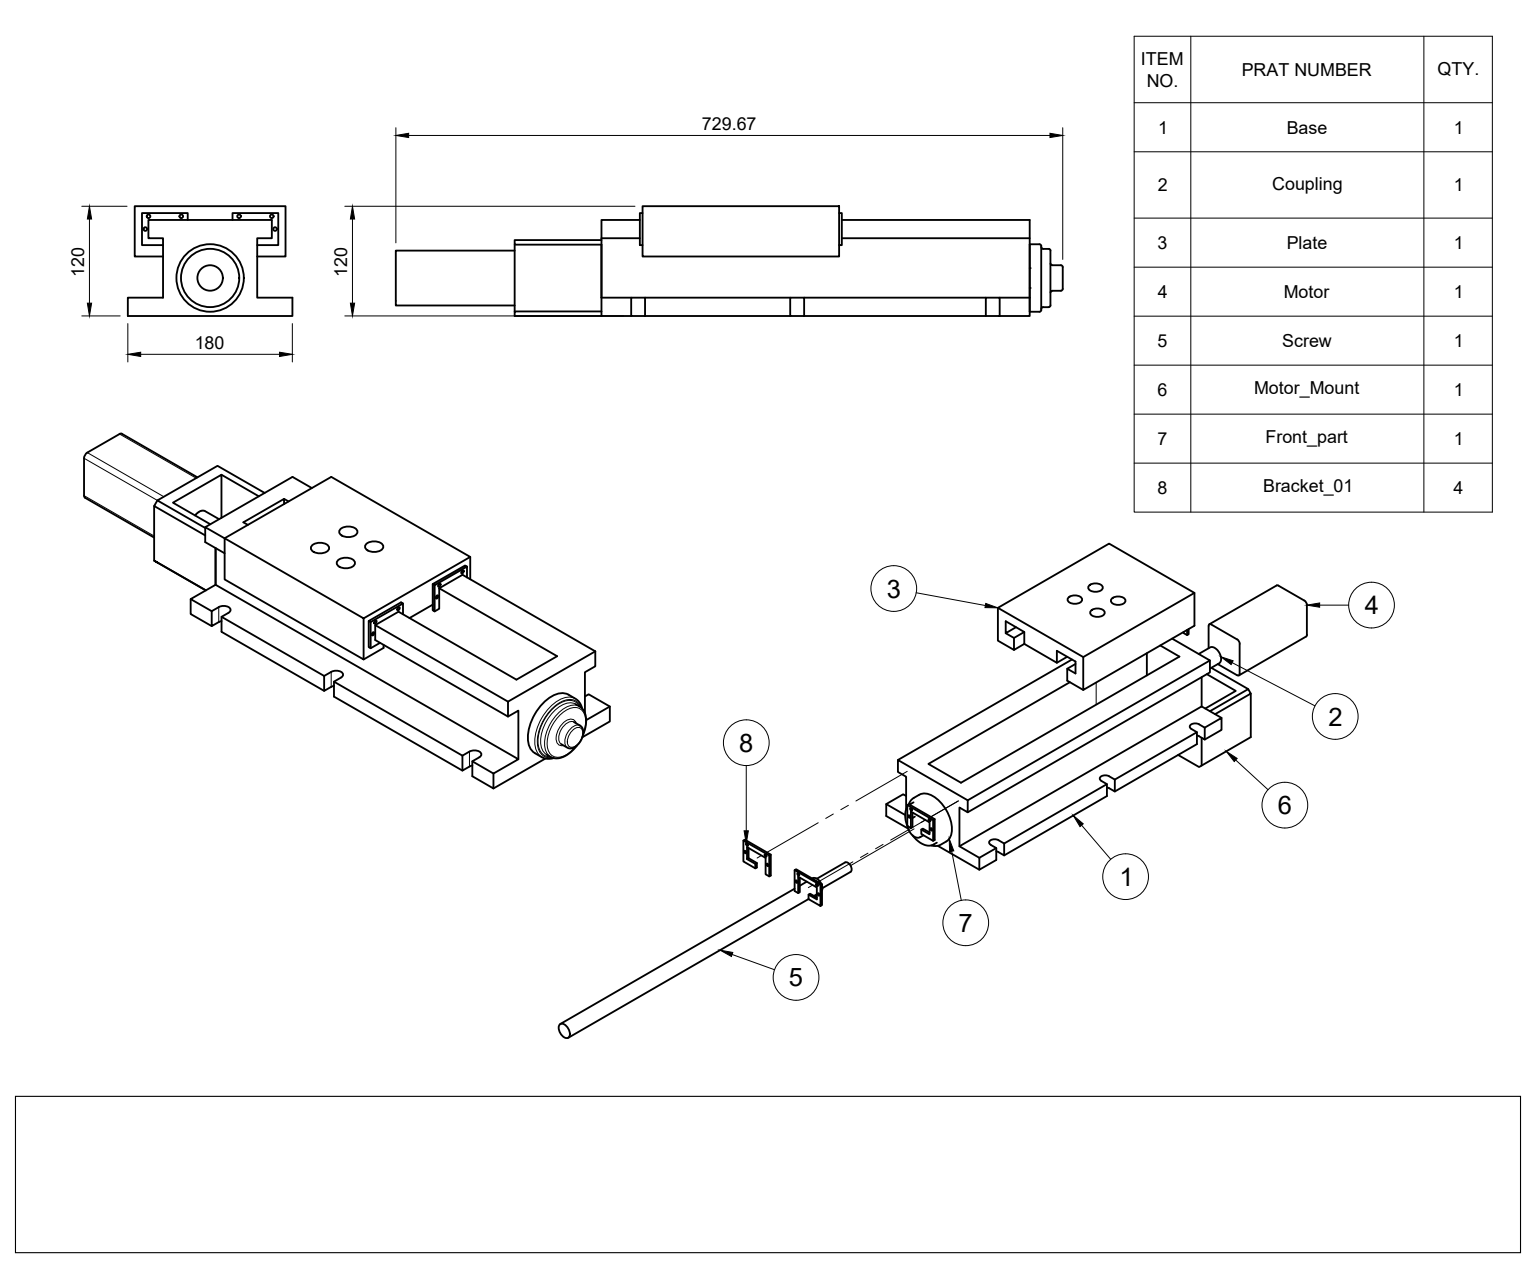
ISO-10303-21;
HEADER;
/* Generated by software containing ST-Developer
 * from STEP Tools, Inc. (www.steptools.com) 
 */

FILE_DESCRIPTION(
/* description */ (''),
/* implementation_level */ '2;1');

FILE_NAME(
/* name */ 'MAS-277',
/* time_stamp */ '2026-10-22T16:03:28+06:00',
/* author */ (''),
/* organization */ (''),
/* preprocessor_version */ 'ST-DEVELOPER v20.2',
/* originating_system */ 'Autodesk Translation Framework v15.15.0.0',
/* authorisation */ '');

FILE_SCHEMA (('AUTOMOTIVE_DESIGN { 1 0 10303 214 3 1 1 }'));
ENDSEC;

DATA;
#10=MECHANICAL_DESIGN_GEOMETRIC_PRESENTATION_REPRESENTATION('',(#84,#85,
#86,#87,#88,#89,#90,#91,#92,#93,#94),#6096);
#11=ITEM_DEFINED_TRANSFORMATION($,$,#3727,#4032);
#12=ITEM_DEFINED_TRANSFORMATION($,$,#3789,#4033);
#13=ITEM_DEFINED_TRANSFORMATION($,$,#3806,#4034);
#14=ITEM_DEFINED_TRANSFORMATION($,$,#3856,#4035);
#15=ITEM_DEFINED_TRANSFORMATION($,$,#3875,#4036);
#16=ITEM_DEFINED_TRANSFORMATION($,$,#3885,#4037);
#17=ITEM_DEFINED_TRANSFORMATION($,$,#3903,#4038);
#18=ITEM_DEFINED_TRANSFORMATION($,$,#3932,#4039);
#19=ITEM_DEFINED_TRANSFORMATION($,$,#3957,#4040);
#20=ITEM_DEFINED_TRANSFORMATION($,$,#3982,#4041);
#21=ITEM_DEFINED_TRANSFORMATION($,$,#4007,#4042);
#22=(
REPRESENTATION_RELATIONSHIP($,$,#6137,#6136)
REPRESENTATION_RELATIONSHIP_WITH_TRANSFORMATION(#11)
SHAPE_REPRESENTATION_RELATIONSHIP()
);
#23=(
REPRESENTATION_RELATIONSHIP($,$,#6138,#6136)
REPRESENTATION_RELATIONSHIP_WITH_TRANSFORMATION(#12)
SHAPE_REPRESENTATION_RELATIONSHIP()
);
#24=(
REPRESENTATION_RELATIONSHIP($,$,#6139,#6136)
REPRESENTATION_RELATIONSHIP_WITH_TRANSFORMATION(#13)
SHAPE_REPRESENTATION_RELATIONSHIP()
);
#25=(
REPRESENTATION_RELATIONSHIP($,$,#6140,#6136)
REPRESENTATION_RELATIONSHIP_WITH_TRANSFORMATION(#14)
SHAPE_REPRESENTATION_RELATIONSHIP()
);
#26=(
REPRESENTATION_RELATIONSHIP($,$,#6141,#6136)
REPRESENTATION_RELATIONSHIP_WITH_TRANSFORMATION(#15)
SHAPE_REPRESENTATION_RELATIONSHIP()
);
#27=(
REPRESENTATION_RELATIONSHIP($,$,#6142,#6136)
REPRESENTATION_RELATIONSHIP_WITH_TRANSFORMATION(#16)
SHAPE_REPRESENTATION_RELATIONSHIP()
);
#28=(
REPRESENTATION_RELATIONSHIP($,$,#6143,#6136)
REPRESENTATION_RELATIONSHIP_WITH_TRANSFORMATION(#17)
SHAPE_REPRESENTATION_RELATIONSHIP()
);
#29=(
REPRESENTATION_RELATIONSHIP($,$,#6144,#6136)
REPRESENTATION_RELATIONSHIP_WITH_TRANSFORMATION(#18)
SHAPE_REPRESENTATION_RELATIONSHIP()
);
#30=(
REPRESENTATION_RELATIONSHIP($,$,#6145,#6136)
REPRESENTATION_RELATIONSHIP_WITH_TRANSFORMATION(#19)
SHAPE_REPRESENTATION_RELATIONSHIP()
);
#31=(
REPRESENTATION_RELATIONSHIP($,$,#6146,#6136)
REPRESENTATION_RELATIONSHIP_WITH_TRANSFORMATION(#20)
SHAPE_REPRESENTATION_RELATIONSHIP()
);
#32=(
REPRESENTATION_RELATIONSHIP($,$,#6147,#6136)
REPRESENTATION_RELATIONSHIP_WITH_TRANSFORMATION(#21)
SHAPE_REPRESENTATION_RELATIONSHIP()
);
#33=CONTEXT_DEPENDENT_SHAPE_REPRESENTATION(#22,#6125);
#34=CONTEXT_DEPENDENT_SHAPE_REPRESENTATION(#23,#6126);
#35=CONTEXT_DEPENDENT_SHAPE_REPRESENTATION(#24,#6127);
#36=CONTEXT_DEPENDENT_SHAPE_REPRESENTATION(#25,#6128);
#37=CONTEXT_DEPENDENT_SHAPE_REPRESENTATION(#26,#6129);
#38=CONTEXT_DEPENDENT_SHAPE_REPRESENTATION(#27,#6130);
#39=CONTEXT_DEPENDENT_SHAPE_REPRESENTATION(#28,#6131);
#40=CONTEXT_DEPENDENT_SHAPE_REPRESENTATION(#29,#6132);
#41=CONTEXT_DEPENDENT_SHAPE_REPRESENTATION(#30,#6133);
#42=CONTEXT_DEPENDENT_SHAPE_REPRESENTATION(#31,#6134);
#43=CONTEXT_DEPENDENT_SHAPE_REPRESENTATION(#32,#6135);
#44=NEXT_ASSEMBLY_USAGE_OCCURRENCE('Base:1','Base:1','Base:1',#6149,#6150,
'Base:1');
#45=NEXT_ASSEMBLY_USAGE_OCCURRENCE('Coupling:1','Coupling:1',
'Coupling:1',#6149,#6151,'Coupling:1');
#46=NEXT_ASSEMBLY_USAGE_OCCURRENCE('Plate:1','Plate:1','Plate:1',#6149,
#6152,'Plate:1');
#47=NEXT_ASSEMBLY_USAGE_OCCURRENCE('Motor:1','Motor:1','Motor:1',#6149,
#6153,'Motor:1');
#48=NEXT_ASSEMBLY_USAGE_OCCURRENCE('Screw:1','Screw:1','Screw:1',#6149,
#6154,'Screw:1');
#49=NEXT_ASSEMBLY_USAGE_OCCURRENCE('Motor_Mount:1','Motor_Mount:1',
'Motor_Mount:1',#6149,#6155,'Motor_Mount:1');
#50=NEXT_ASSEMBLY_USAGE_OCCURRENCE('Front_part:1','Front_part:1',
'Front_part:1',#6149,#6156,'Front_part:1');
#51=NEXT_ASSEMBLY_USAGE_OCCURRENCE('Bracket_01:1','Bracket_01:1',
'Bracket_01:1',#6149,#6157,'Bracket_01:1');
#52=NEXT_ASSEMBLY_USAGE_OCCURRENCE('Bracket_02:1','Bracket_02:1',
'Bracket_02:1',#6149,#6158,'Bracket_02:1');
#53=NEXT_ASSEMBLY_USAGE_OCCURRENCE('Bracket_03:1','Bracket_03:1',
'Bracket_03:1',#6149,#6159,'Bracket_03:1');
#54=NEXT_ASSEMBLY_USAGE_OCCURRENCE('Bracket_04:1','Bracket_04:1',
'Bracket_04:1',#6149,#6160,'Bracket_04:1');
#55=TOROIDAL_SURFACE('',#3790,12.,0.5);
#56=TOROIDAL_SURFACE('',#3800,12.,0.5);
#57=TOROIDAL_SURFACE('',#3904,33.837899857748,2.);
#58=TOROIDAL_SURFACE('',#3912,15.946575006305,2.);
#59=TOROIDAL_SURFACE('',#3920,11.946575006305,2.);
#60=TOROIDAL_SURFACE('',#3924,29.837899857748,2.);
#61=TOROIDAL_SURFACE('',#3926,34.8878705819456,2.);
#62=SHAPE_REPRESENTATION_RELATIONSHIP('SRR','None',#6137,#73);
#63=SHAPE_REPRESENTATION_RELATIONSHIP('SRR','None',#6138,#74);
#64=SHAPE_REPRESENTATION_RELATIONSHIP('SRR','None',#6139,#75);
#65=SHAPE_REPRESENTATION_RELATIONSHIP('SRR','None',#6140,#76);
#66=SHAPE_REPRESENTATION_RELATIONSHIP('SRR','None',#6141,#77);
#67=SHAPE_REPRESENTATION_RELATIONSHIP('SRR','None',#6142,#78);
#68=SHAPE_REPRESENTATION_RELATIONSHIP('SRR','None',#6143,#79);
#69=SHAPE_REPRESENTATION_RELATIONSHIP('SRR','None',#6144,#80);
#70=SHAPE_REPRESENTATION_RELATIONSHIP('SRR','None',#6145,#81);
#71=SHAPE_REPRESENTATION_RELATIONSHIP('SRR','None',#6146,#82);
#72=SHAPE_REPRESENTATION_RELATIONSHIP('SRR','None',#6147,#83);
#73=ADVANCED_BREP_SHAPE_REPRESENTATION('',(#95),#6085);
#74=ADVANCED_BREP_SHAPE_REPRESENTATION('',(#96),#6086);
#75=ADVANCED_BREP_SHAPE_REPRESENTATION('',(#97),#6087);
#76=ADVANCED_BREP_SHAPE_REPRESENTATION('',(#98),#6088);
#77=ADVANCED_BREP_SHAPE_REPRESENTATION('',(#99),#6089);
#78=ADVANCED_BREP_SHAPE_REPRESENTATION('',(#100),#6090);
#79=ADVANCED_BREP_SHAPE_REPRESENTATION('',(#101),#6091);
#80=ADVANCED_BREP_SHAPE_REPRESENTATION('',(#102),#6092);
#81=ADVANCED_BREP_SHAPE_REPRESENTATION('',(#103),#6093);
#82=ADVANCED_BREP_SHAPE_REPRESENTATION('',(#104),#6094);
#83=ADVANCED_BREP_SHAPE_REPRESENTATION('',(#105),#6095);
#84=STYLED_ITEM('',(#6234),#95);
#85=STYLED_ITEM('',(#6248),#96);
#86=STYLED_ITEM('',(#6269),#97);
#87=STYLED_ITEM('',(#6269),#98);
#88=STYLED_ITEM('',(#6262),#99);
#89=STYLED_ITEM('',(#6269),#100);
#90=STYLED_ITEM('',(#6248),#101);
#91=STYLED_ITEM('',(#6234),#102);
#92=STYLED_ITEM('',(#6234),#103);
#93=STYLED_ITEM('',(#6234),#104);
#94=STYLED_ITEM('',(#6234),#105);
#95=MANIFOLD_SOLID_BREP('Base',#3593);
#96=MANIFOLD_SOLID_BREP('Coupling',#3594);
#97=MANIFOLD_SOLID_BREP('Plate',#3595);
#98=MANIFOLD_SOLID_BREP('Motor',#3596);
#99=MANIFOLD_SOLID_BREP('Screw',#3597);
#100=MANIFOLD_SOLID_BREP('Motor_Mount',#3598);
#101=MANIFOLD_SOLID_BREP('Front_part',#3599);
#102=MANIFOLD_SOLID_BREP('Bracket_01',#3600);
#103=MANIFOLD_SOLID_BREP('Bracket_02',#3601);
#104=MANIFOLD_SOLID_BREP('Bracket_03',#3602);
#105=MANIFOLD_SOLID_BREP('Bracket_04',#3603);
#106=FACE_BOUND('',#517,.T.);
#107=FACE_BOUND('',#522,.T.);
#108=FACE_BOUND('',#524,.T.);
#109=FACE_BOUND('',#529,.T.);
#110=FACE_BOUND('',#535,.T.);
#111=FACE_BOUND('',#539,.T.);
#112=FACE_BOUND('',#542,.T.);
#113=FACE_BOUND('',#546,.T.);
#114=FACE_BOUND('',#548,.T.);
#115=FACE_BOUND('',#574,.T.);
#116=FACE_BOUND('',#575,.T.);
#117=FACE_BOUND('',#576,.T.);
#118=FACE_BOUND('',#577,.T.);
#119=FACE_BOUND('',#595,.T.);
#120=FACE_BOUND('',#601,.T.);
#121=FACE_BOUND('',#605,.T.);
#122=FACE_BOUND('',#607,.T.);
#123=FACE_BOUND('',#610,.T.);
#124=FACE_BOUND('',#619,.T.);
#125=FACE_BOUND('',#623,.T.);
#126=FACE_BOUND('',#645,.T.);
#127=FACE_BOUND('',#646,.T.);
#128=FACE_BOUND('',#647,.T.);
#129=FACE_BOUND('',#648,.T.);
#130=FACE_BOUND('',#650,.T.);
#131=FACE_BOUND('',#651,.T.);
#132=FACE_BOUND('',#652,.T.);
#133=FACE_BOUND('',#653,.T.);
#134=FACE_BOUND('',#669,.T.);
#135=FACE_BOUND('',#670,.T.);
#136=FACE_BOUND('',#671,.T.);
#137=FACE_BOUND('',#672,.T.);
#138=FACE_BOUND('',#674,.T.);
#139=FACE_BOUND('',#675,.T.);
#140=FACE_BOUND('',#676,.T.);
#141=FACE_BOUND('',#677,.T.);
#142=FACE_BOUND('',#693,.T.);
#143=FACE_BOUND('',#694,.T.);
#144=FACE_BOUND('',#695,.T.);
#145=FACE_BOUND('',#696,.T.);
#146=FACE_BOUND('',#698,.T.);
#147=FACE_BOUND('',#699,.T.);
#148=FACE_BOUND('',#700,.T.);
#149=FACE_BOUND('',#701,.T.);
#150=FACE_BOUND('',#717,.T.);
#151=FACE_BOUND('',#718,.T.);
#152=FACE_BOUND('',#719,.T.);
#153=FACE_BOUND('',#720,.T.);
#154=FACE_BOUND('',#722,.T.);
#155=FACE_BOUND('',#723,.T.);
#156=FACE_BOUND('',#724,.T.);
#157=FACE_BOUND('',#725,.T.);
#158=PLANE('',#3734);
#159=PLANE('',#3738);
#160=PLANE('',#3739);
#161=PLANE('',#3743);
#162=PLANE('',#3744);
#163=PLANE('',#3748);
#164=PLANE('',#3749);
#165=PLANE('',#3750);
#166=PLANE('',#3751);
#167=PLANE('',#3752);
#168=PLANE('',#3753);
#169=PLANE('',#3754);
#170=PLANE('',#3755);
#171=PLANE('',#3759);
#172=PLANE('',#3760);
#173=PLANE('',#3764);
#174=PLANE('',#3765);
#175=PLANE('',#3769);
#176=PLANE('',#3770);
#177=PLANE('',#3771);
#178=PLANE('',#3772);
#179=PLANE('',#3773);
#180=PLANE('',#3774);
#181=PLANE('',#3775);
#182=PLANE('',#3776);
#183=PLANE('',#3777);
#184=PLANE('',#3778);
#185=PLANE('',#3779);
#186=PLANE('',#3780);
#187=PLANE('',#3781);
#188=PLANE('',#3782);
#189=PLANE('',#3783);
#190=PLANE('',#3784);
#191=PLANE('',#3785);
#192=PLANE('',#3786);
#193=PLANE('',#3787);
#194=PLANE('',#3788);
#195=PLANE('',#3798);
#196=PLANE('',#3803);
#197=PLANE('',#3810);
#198=PLANE('',#3811);
#199=PLANE('',#3812);
#200=PLANE('',#3813);
#201=PLANE('',#3814);
#202=PLANE('',#3815);
#203=PLANE('',#3817);
#204=PLANE('',#3820);
#205=PLANE('',#3823);
#206=PLANE('',#3825);
#207=PLANE('',#3826);
#208=PLANE('',#3827);
#209=PLANE('',#3830);
#210=PLANE('',#3843);
#211=PLANE('',#3844);
#212=PLANE('',#3845);
#213=PLANE('',#3846);
#214=PLANE('',#3847);
#215=PLANE('',#3848);
#216=PLANE('',#3849);
#217=PLANE('',#3850);
#218=PLANE('',#3851);
#219=PLANE('',#3852);
#220=PLANE('',#3853);
#221=PLANE('',#3854);
#222=PLANE('',#3855);
#223=PLANE('',#3860);
#224=PLANE('',#3864);
#225=PLANE('',#3869);
#226=PLANE('',#3872);
#227=PLANE('',#3873);
#228=PLANE('',#3874);
#229=PLANE('',#3879);
#230=PLANE('',#3883);
#231=PLANE('',#3884);
#232=PLANE('',#3889);
#233=PLANE('',#3890);
#234=PLANE('',#3891);
#235=PLANE('',#3892);
#236=PLANE('',#3893);
#237=PLANE('',#3894);
#238=PLANE('',#3895);
#239=PLANE('',#3896);
#240=PLANE('',#3897);
#241=PLANE('',#3898);
#242=PLANE('',#3899);
#243=PLANE('',#3900);
#244=PLANE('',#3901);
#245=PLANE('',#3902);
#246=PLANE('',#3910);
#247=PLANE('',#3918);
#248=PLANE('',#3923);
#249=PLANE('',#3931);
#250=PLANE('',#3945);
#251=PLANE('',#3946);
#252=PLANE('',#3947);
#253=PLANE('',#3948);
#254=PLANE('',#3949);
#255=PLANE('',#3950);
#256=PLANE('',#3951);
#257=PLANE('',#3952);
#258=PLANE('',#3953);
#259=PLANE('',#3954);
#260=PLANE('',#3955);
#261=PLANE('',#3956);
#262=PLANE('',#3970);
#263=PLANE('',#3971);
#264=PLANE('',#3972);
#265=PLANE('',#3973);
#266=PLANE('',#3974);
#267=PLANE('',#3975);
#268=PLANE('',#3976);
#269=PLANE('',#3977);
#270=PLANE('',#3978);
#271=PLANE('',#3979);
#272=PLANE('',#3980);
#273=PLANE('',#3981);
#274=PLANE('',#3995);
#275=PLANE('',#3996);
#276=PLANE('',#3997);
#277=PLANE('',#3998);
#278=PLANE('',#3999);
#279=PLANE('',#4000);
#280=PLANE('',#4001);
#281=PLANE('',#4002);
#282=PLANE('',#4003);
#283=PLANE('',#4004);
#284=PLANE('',#4005);
#285=PLANE('',#4006);
#286=PLANE('',#4020);
#287=PLANE('',#4021);
#288=PLANE('',#4022);
#289=PLANE('',#4023);
#290=PLANE('',#4024);
#291=PLANE('',#4025);
#292=PLANE('',#4026);
#293=PLANE('',#4027);
#294=PLANE('',#4028);
#295=PLANE('',#4029);
#296=PLANE('',#4030);
#297=PLANE('',#4031);
#298=FACE_OUTER_BOUND('',#486,.T.);
#299=FACE_OUTER_BOUND('',#487,.T.);
#300=FACE_OUTER_BOUND('',#488,.T.);
#301=FACE_OUTER_BOUND('',#489,.T.);
#302=FACE_OUTER_BOUND('',#490,.T.);
#303=FACE_OUTER_BOUND('',#491,.T.);
#304=FACE_OUTER_BOUND('',#492,.T.);
#305=FACE_OUTER_BOUND('',#493,.T.);
#306=FACE_OUTER_BOUND('',#494,.T.);
#307=FACE_OUTER_BOUND('',#495,.T.);
#308=FACE_OUTER_BOUND('',#496,.T.);
#309=FACE_OUTER_BOUND('',#497,.T.);
#310=FACE_OUTER_BOUND('',#498,.T.);
#311=FACE_OUTER_BOUND('',#499,.T.);
#312=FACE_OUTER_BOUND('',#500,.T.);
#313=FACE_OUTER_BOUND('',#501,.T.);
#314=FACE_OUTER_BOUND('',#502,.T.);
#315=FACE_OUTER_BOUND('',#503,.T.);
#316=FACE_OUTER_BOUND('',#504,.T.);
#317=FACE_OUTER_BOUND('',#505,.T.);
#318=FACE_OUTER_BOUND('',#506,.T.);
#319=FACE_OUTER_BOUND('',#507,.T.);
#320=FACE_OUTER_BOUND('',#508,.T.);
#321=FACE_OUTER_BOUND('',#509,.T.);
#322=FACE_OUTER_BOUND('',#510,.T.);
#323=FACE_OUTER_BOUND('',#511,.T.);
#324=FACE_OUTER_BOUND('',#512,.T.);
#325=FACE_OUTER_BOUND('',#513,.T.);
#326=FACE_OUTER_BOUND('',#514,.T.);
#327=FACE_OUTER_BOUND('',#515,.T.);
#328=FACE_OUTER_BOUND('',#516,.T.);
#329=FACE_OUTER_BOUND('',#518,.T.);
#330=FACE_OUTER_BOUND('',#519,.T.);
#331=FACE_OUTER_BOUND('',#520,.T.);
#332=FACE_OUTER_BOUND('',#521,.T.);
#333=FACE_OUTER_BOUND('',#523,.T.);
#334=FACE_OUTER_BOUND('',#525,.T.);
#335=FACE_OUTER_BOUND('',#526,.T.);
#336=FACE_OUTER_BOUND('',#527,.T.);
#337=FACE_OUTER_BOUND('',#528,.T.);
#338=FACE_OUTER_BOUND('',#530,.T.);
#339=FACE_OUTER_BOUND('',#531,.T.);
#340=FACE_OUTER_BOUND('',#532,.T.);
#341=FACE_OUTER_BOUND('',#533,.T.);
#342=FACE_OUTER_BOUND('',#534,.T.);
#343=FACE_OUTER_BOUND('',#536,.T.);
#344=FACE_OUTER_BOUND('',#537,.T.);
#345=FACE_OUTER_BOUND('',#538,.T.);
#346=FACE_OUTER_BOUND('',#540,.T.);
#347=FACE_OUTER_BOUND('',#541,.T.);
#348=FACE_OUTER_BOUND('',#543,.T.);
#349=FACE_OUTER_BOUND('',#544,.T.);
#350=FACE_OUTER_BOUND('',#545,.T.);
#351=FACE_OUTER_BOUND('',#547,.T.);
#352=FACE_OUTER_BOUND('',#549,.T.);
#353=FACE_OUTER_BOUND('',#550,.T.);
#354=FACE_OUTER_BOUND('',#551,.T.);
#355=FACE_OUTER_BOUND('',#552,.T.);
#356=FACE_OUTER_BOUND('',#553,.T.);
#357=FACE_OUTER_BOUND('',#554,.T.);
#358=FACE_OUTER_BOUND('',#555,.T.);
#359=FACE_OUTER_BOUND('',#556,.T.);
#360=FACE_OUTER_BOUND('',#557,.T.);
#361=FACE_OUTER_BOUND('',#558,.T.);
#362=FACE_OUTER_BOUND('',#559,.T.);
#363=FACE_OUTER_BOUND('',#560,.T.);
#364=FACE_OUTER_BOUND('',#561,.T.);
#365=FACE_OUTER_BOUND('',#562,.T.);
#366=FACE_OUTER_BOUND('',#563,.T.);
#367=FACE_OUTER_BOUND('',#564,.T.);
#368=FACE_OUTER_BOUND('',#565,.T.);
#369=FACE_OUTER_BOUND('',#566,.T.);
#370=FACE_OUTER_BOUND('',#567,.T.);
#371=FACE_OUTER_BOUND('',#568,.T.);
#372=FACE_OUTER_BOUND('',#569,.T.);
#373=FACE_OUTER_BOUND('',#570,.T.);
#374=FACE_OUTER_BOUND('',#571,.T.);
#375=FACE_OUTER_BOUND('',#572,.T.);
#376=FACE_OUTER_BOUND('',#573,.T.);
#377=FACE_OUTER_BOUND('',#578,.T.);
#378=FACE_OUTER_BOUND('',#579,.T.);
#379=FACE_OUTER_BOUND('',#580,.T.);
#380=FACE_OUTER_BOUND('',#581,.T.);
#381=FACE_OUTER_BOUND('',#582,.T.);
#382=FACE_OUTER_BOUND('',#583,.T.);
#383=FACE_OUTER_BOUND('',#584,.T.);
#384=FACE_OUTER_BOUND('',#585,.T.);
#385=FACE_OUTER_BOUND('',#586,.T.);
#386=FACE_OUTER_BOUND('',#587,.T.);
#387=FACE_OUTER_BOUND('',#588,.T.);
#388=FACE_OUTER_BOUND('',#589,.T.);
#389=FACE_OUTER_BOUND('',#590,.T.);
#390=FACE_OUTER_BOUND('',#591,.T.);
#391=FACE_OUTER_BOUND('',#592,.T.);
#392=FACE_OUTER_BOUND('',#593,.T.);
#393=FACE_OUTER_BOUND('',#594,.T.);
#394=FACE_OUTER_BOUND('',#596,.T.);
#395=FACE_OUTER_BOUND('',#597,.T.);
#396=FACE_OUTER_BOUND('',#598,.T.);
#397=FACE_OUTER_BOUND('',#599,.T.);
#398=FACE_OUTER_BOUND('',#600,.T.);
#399=FACE_OUTER_BOUND('',#602,.T.);
#400=FACE_OUTER_BOUND('',#603,.T.);
#401=FACE_OUTER_BOUND('',#604,.T.);
#402=FACE_OUTER_BOUND('',#606,.T.);
#403=FACE_OUTER_BOUND('',#608,.T.);
#404=FACE_OUTER_BOUND('',#609,.T.);
#405=FACE_OUTER_BOUND('',#611,.T.);
#406=FACE_OUTER_BOUND('',#612,.T.);
#407=FACE_OUTER_BOUND('',#613,.T.);
#408=FACE_OUTER_BOUND('',#614,.T.);
#409=FACE_OUTER_BOUND('',#615,.T.);
#410=FACE_OUTER_BOUND('',#616,.T.);
#411=FACE_OUTER_BOUND('',#617,.T.);
#412=FACE_OUTER_BOUND('',#618,.T.);
#413=FACE_OUTER_BOUND('',#620,.T.);
#414=FACE_OUTER_BOUND('',#621,.T.);
#415=FACE_OUTER_BOUND('',#622,.T.);
#416=FACE_OUTER_BOUND('',#624,.T.);
#417=FACE_OUTER_BOUND('',#625,.T.);
#418=FACE_OUTER_BOUND('',#626,.T.);
#419=FACE_OUTER_BOUND('',#627,.T.);
#420=FACE_OUTER_BOUND('',#628,.T.);
#421=FACE_OUTER_BOUND('',#629,.T.);
#422=FACE_OUTER_BOUND('',#630,.T.);
#423=FACE_OUTER_BOUND('',#631,.T.);
#424=FACE_OUTER_BOUND('',#632,.T.);
#425=FACE_OUTER_BOUND('',#633,.T.);
#426=FACE_OUTER_BOUND('',#634,.T.);
#427=FACE_OUTER_BOUND('',#635,.T.);
#428=FACE_OUTER_BOUND('',#636,.T.);
#429=FACE_OUTER_BOUND('',#637,.T.);
#430=FACE_OUTER_BOUND('',#638,.T.);
#431=FACE_OUTER_BOUND('',#639,.T.);
#432=FACE_OUTER_BOUND('',#640,.T.);
#433=FACE_OUTER_BOUND('',#641,.T.);
#434=FACE_OUTER_BOUND('',#642,.T.);
#435=FACE_OUTER_BOUND('',#643,.T.);
#436=FACE_OUTER_BOUND('',#644,.T.);
#437=FACE_OUTER_BOUND('',#649,.T.);
#438=FACE_OUTER_BOUND('',#654,.T.);
#439=FACE_OUTER_BOUND('',#655,.T.);
#440=FACE_OUTER_BOUND('',#656,.T.);
#441=FACE_OUTER_BOUND('',#657,.T.);
#442=FACE_OUTER_BOUND('',#658,.T.);
#443=FACE_OUTER_BOUND('',#659,.T.);
#444=FACE_OUTER_BOUND('',#660,.T.);
#445=FACE_OUTER_BOUND('',#661,.T.);
#446=FACE_OUTER_BOUND('',#662,.T.);
#447=FACE_OUTER_BOUND('',#663,.T.);
#448=FACE_OUTER_BOUND('',#664,.T.);
#449=FACE_OUTER_BOUND('',#665,.T.);
#450=FACE_OUTER_BOUND('',#666,.T.);
#451=FACE_OUTER_BOUND('',#667,.T.);
#452=FACE_OUTER_BOUND('',#668,.T.);
#453=FACE_OUTER_BOUND('',#673,.T.);
#454=FACE_OUTER_BOUND('',#678,.T.);
#455=FACE_OUTER_BOUND('',#679,.T.);
#456=FACE_OUTER_BOUND('',#680,.T.);
#457=FACE_OUTER_BOUND('',#681,.T.);
#458=FACE_OUTER_BOUND('',#682,.T.);
#459=FACE_OUTER_BOUND('',#683,.T.);
#460=FACE_OUTER_BOUND('',#684,.T.);
#461=FACE_OUTER_BOUND('',#685,.T.);
#462=FACE_OUTER_BOUND('',#686,.T.);
#463=FACE_OUTER_BOUND('',#687,.T.);
#464=FACE_OUTER_BOUND('',#688,.T.);
#465=FACE_OUTER_BOUND('',#689,.T.);
#466=FACE_OUTER_BOUND('',#690,.T.);
#467=FACE_OUTER_BOUND('',#691,.T.);
#468=FACE_OUTER_BOUND('',#692,.T.);
#469=FACE_OUTER_BOUND('',#697,.T.);
#470=FACE_OUTER_BOUND('',#702,.T.);
#471=FACE_OUTER_BOUND('',#703,.T.);
#472=FACE_OUTER_BOUND('',#704,.T.);
#473=FACE_OUTER_BOUND('',#705,.T.);
#474=FACE_OUTER_BOUND('',#706,.T.);
#475=FACE_OUTER_BOUND('',#707,.T.);
#476=FACE_OUTER_BOUND('',#708,.T.);
#477=FACE_OUTER_BOUND('',#709,.T.);
#478=FACE_OUTER_BOUND('',#710,.T.);
#479=FACE_OUTER_BOUND('',#711,.T.);
#480=FACE_OUTER_BOUND('',#712,.T.);
#481=FACE_OUTER_BOUND('',#713,.T.);
#482=FACE_OUTER_BOUND('',#714,.T.);
#483=FACE_OUTER_BOUND('',#715,.T.);
#484=FACE_OUTER_BOUND('',#716,.T.);
#485=FACE_OUTER_BOUND('',#721,.T.);
#486=EDGE_LOOP('',(#2394,#2395,#2396,#2397));
#487=EDGE_LOOP('',(#2398,#2399,#2400,#2401));
#488=EDGE_LOOP('',(#2402,#2403,#2404,#2405));
#489=EDGE_LOOP('',(#2406,#2407,#2408,#2409));
#490=EDGE_LOOP('',(#2410,#2411,#2412,#2413));
#491=EDGE_LOOP('',(#2414,#2415,#2416,#2417));
#492=EDGE_LOOP('',(#2418,#2419,#2420,#2421));
#493=EDGE_LOOP('',(#2422,#2423,#2424,#2425));
#494=EDGE_LOOP('',(#2426,#2427,#2428,#2429));
#495=EDGE_LOOP('',(#2430,#2431,#2432,#2433));
#496=EDGE_LOOP('',(#2434,#2435,#2436,#2437));
#497=EDGE_LOOP('',(#2438,#2439,#2440,#2441,#2442,#2443,#2444,#2445,#2446,
#2447,#2448,#2449,#2450,#2451,#2452,#2453));
#498=EDGE_LOOP('',(#2454,#2455,#2456,#2457));
#499=EDGE_LOOP('',(#2458,#2459,#2460,#2461));
#500=EDGE_LOOP('',(#2462,#2463,#2464,#2465));
#501=EDGE_LOOP('',(#2466,#2467,#2468,#2469));
#502=EDGE_LOOP('',(#2470,#2471,#2472,#2473));
#503=EDGE_LOOP('',(#2474,#2475,#2476,#2477));
#504=EDGE_LOOP('',(#2478,#2479,#2480,#2481));
#505=EDGE_LOOP('',(#2482,#2483,#2484,#2485));
#506=EDGE_LOOP('',(#2486,#2487,#2488,#2489));
#507=EDGE_LOOP('',(#2490,#2491,#2492,#2493));
#508=EDGE_LOOP('',(#2494,#2495,#2496,#2497));
#509=EDGE_LOOP('',(#2498,#2499,#2500,#2501));
#510=EDGE_LOOP('',(#2502,#2503,#2504,#2505));
#511=EDGE_LOOP('',(#2506,#2507,#2508,#2509));
#512=EDGE_LOOP('',(#2510,#2511,#2512,#2513));
#513=EDGE_LOOP('',(#2514,#2515,#2516,#2517));
#514=EDGE_LOOP('',(#2518,#2519,#2520,#2521));
#515=EDGE_LOOP('',(#2522,#2523,#2524,#2525,#2526,#2527,#2528,#2529,#2530,
#2531,#2532,#2533,#2534,#2535,#2536,#2537,#2538,#2539,#2540,#2541,#2542,
#2543,#2544,#2545,#2546,#2547,#2548,#2549));
#516=EDGE_LOOP('',(#2550,#2551,#2552,#2553));
#517=EDGE_LOOP('',(#2554));
#518=EDGE_LOOP('',(#2555,#2556,#2557,#2558));
#519=EDGE_LOOP('',(#2559,#2560,#2561,#2562));
#520=EDGE_LOOP('',(#2563,#2564,#2565,#2566));
#521=EDGE_LOOP('',(#2567,#2568,#2569,#2570));
#522=EDGE_LOOP('',(#2571));
#523=EDGE_LOOP('',(#2572,#2573,#2574,#2575,#2576,#2577,#2578,#2579,#2580,
#2581,#2582,#2583));
#524=EDGE_LOOP('',(#2584));
#525=EDGE_LOOP('',(#2585,#2586,#2587,#2588));
#526=EDGE_LOOP('',(#2589,#2590,#2591,#2592));
#527=EDGE_LOOP('',(#2593,#2594,#2595,#2596));
#528=EDGE_LOOP('',(#2597,#2598,#2599,#2600));
#529=EDGE_LOOP('',(#2601,#2602,#2603,#2604));
#530=EDGE_LOOP('',(#2605,#2606,#2607,#2608,#2609,#2610,#2611,#2612,#2613,
#2614,#2615,#2616,#2617,#2618,#2619,#2620));
#531=EDGE_LOOP('',(#2621,#2622,#2623,#2624));
#532=EDGE_LOOP('',(#2625,#2626,#2627,#2628));
#533=EDGE_LOOP('',(#2629,#2630,#2631,#2632));
#534=EDGE_LOOP('',(#2633,#2634,#2635,#2636,#2637,#2638,#2639,#2640,#2641,
#2642,#2643,#2644));
#535=EDGE_LOOP('',(#2645));
#536=EDGE_LOOP('',(#2646,#2647,#2648,#2649,#2650));
#537=EDGE_LOOP('',(#2651,#2652,#2653,#2654,#2655,#2656));
#538=EDGE_LOOP('',(#2657));
#539=EDGE_LOOP('',(#2658));
#540=EDGE_LOOP('',(#2659,#2660,#2661,#2662,#2663));
#541=EDGE_LOOP('',(#2664));
#542=EDGE_LOOP('',(#2665));
#543=EDGE_LOOP('',(#2666,#2667,#2668,#2669));
#544=EDGE_LOOP('',(#2670,#2671,#2672,#2673));
#545=EDGE_LOOP('',(#2674,#2675,#2676,#2677));
#546=EDGE_LOOP('',(#2678));
#547=EDGE_LOOP('',(#2679,#2680,#2681,#2682));
#548=EDGE_LOOP('',(#2683));
#549=EDGE_LOOP('',(#2684,#2685,#2686,#2687));
#550=EDGE_LOOP('',(#2688,#2689,#2690,#2691));
#551=EDGE_LOOP('',(#2692,#2693,#2694,#2695));
#552=EDGE_LOOP('',(#2696,#2697));
#553=EDGE_LOOP('',(#2698,#2699,#2700));
#554=EDGE_LOOP('',(#2701,#2702,#2703));
#555=EDGE_LOOP('',(#2704,#2705));
#556=EDGE_LOOP('',(#2706,#2707,#2708,#2709,#2710,#2711,#2712,#2713,#2714,
#2715,#2716,#2717));
#557=EDGE_LOOP('',(#2718,#2719,#2720,#2721,#2722,#2723,#2724,#2725,#2726,
#2727,#2728,#2729));
#558=EDGE_LOOP('',(#2730,#2731,#2732,#2733,#2734,#2735,#2736,#2737));
#559=EDGE_LOOP('',(#2738,#2739,#2740,#2741,#2742,#2743,#2744,#2745,#2746,
#2747));
#560=EDGE_LOOP('',(#2748,#2749,#2750,#2751,#2752,#2753));
#561=EDGE_LOOP('',(#2754,#2755,#2756,#2757,#2758,#2759));
#562=EDGE_LOOP('',(#2760,#2761,#2762,#2763,#2764,#2765));
#563=EDGE_LOOP('',(#2766,#2767,#2768,#2769,#2770,#2771));
#564=EDGE_LOOP('',(#2772,#2773,#2774,#2775));
#565=EDGE_LOOP('',(#2776,#2777,#2778,#2779));
#566=EDGE_LOOP('',(#2780,#2781,#2782,#2783));
#567=EDGE_LOOP('',(#2784,#2785,#2786,#2787));
#568=EDGE_LOOP('',(#2788,#2789,#2790,#2791));
#569=EDGE_LOOP('',(#2792,#2793,#2794,#2795,#2796,#2797,#2798,#2799,#2800,
#2801,#2802,#2803,#2804,#2805,#2806,#2807));
#570=EDGE_LOOP('',(#2808,#2809,#2810,#2811));
#571=EDGE_LOOP('',(#2812,#2813,#2814,#2815));
#572=EDGE_LOOP('',(#2816,#2817,#2818,#2819));
#573=EDGE_LOOP('',(#2820,#2821,#2822,#2823));
#574=EDGE_LOOP('',(#2824));
#575=EDGE_LOOP('',(#2825));
#576=EDGE_LOOP('',(#2826));
#577=EDGE_LOOP('',(#2827));
#578=EDGE_LOOP('',(#2828,#2829,#2830,#2831));
#579=EDGE_LOOP('',(#2832,#2833,#2834,#2835));
#580=EDGE_LOOP('',(#2836,#2837,#2838,#2839,#2840,#2841,#2842,#2843,#2844,
#2845,#2846,#2847,#2848,#2849,#2850,#2851));
#581=EDGE_LOOP('',(#2852,#2853,#2854,#2855));
#582=EDGE_LOOP('',(#2856,#2857,#2858,#2859,#2860,#2861,#2862,#2863));
#583=EDGE_LOOP('',(#2864,#2865,#2866,#2867));
#584=EDGE_LOOP('',(#2868,#2869,#2870,#2871));
#585=EDGE_LOOP('',(#2872,#2873,#2874,#2875));
#586=EDGE_LOOP('',(#2876,#2877,#2878,#2879));
#587=EDGE_LOOP('',(#2880,#2881,#2882,#2883));
#588=EDGE_LOOP('',(#2884,#2885,#2886,#2887));
#589=EDGE_LOOP('',(#2888,#2889,#2890,#2891));
#590=EDGE_LOOP('',(#2892,#2893,#2894,#2895,#2896,#2897,#2898,#2899));
#591=EDGE_LOOP('',(#2900,#2901,#2902,#2903));
#592=EDGE_LOOP('',(#2904));
#593=EDGE_LOOP('',(#2905,#2906,#2907,#2908));
#594=EDGE_LOOP('',(#2909));
#595=EDGE_LOOP('',(#2910));
#596=EDGE_LOOP('',(#2911));
#597=EDGE_LOOP('',(#2912,#2913,#2914,#2915));
#598=EDGE_LOOP('',(#2916,#2917,#2918,#2919));
#599=EDGE_LOOP('',(#2920,#2921,#2922,#2923));
#600=EDGE_LOOP('',(#2924,#2925,#2926,#2927));
#601=EDGE_LOOP('',(#2928));
#602=EDGE_LOOP('',(#2929,#2930,#2931,#2932));
#603=EDGE_LOOP('',(#2933,#2934,#2935,#2936));
#604=EDGE_LOOP('',(#2937,#2938,#2939,#2940));
#605=EDGE_LOOP('',(#2941,#2942,#2943,#2944));
#606=EDGE_LOOP('',(#2945,#2946,#2947,#2948,#2949,#2950,#2951,#2952));
#607=EDGE_LOOP('',(#2953));
#608=EDGE_LOOP('',(#2954,#2955,#2956,#2957));
#609=EDGE_LOOP('',(#2958,#2959,#2960,#2961));
#610=EDGE_LOOP('',(#2962,#2963,#2964,#2965));
#611=EDGE_LOOP('',(#2966,#2967,#2968,#2969));
#612=EDGE_LOOP('',(#2970,#2971,#2972,#2973));
#613=EDGE_LOOP('',(#2974,#2975,#2976,#2977));
#614=EDGE_LOOP('',(#2978,#2979,#2980,#2981));
#615=EDGE_LOOP('',(#2982,#2983,#2984,#2985,#2986,#2987,#2988,#2989));
#616=EDGE_LOOP('',(#2990,#2991,#2992,#2993));
#617=EDGE_LOOP('',(#2994,#2995,#2996,#2997));
#618=EDGE_LOOP('',(#2998));
#619=EDGE_LOOP('',(#2999));
#620=EDGE_LOOP('',(#3000,#3001,#3002,#3003));
#621=EDGE_LOOP('',(#3004,#3005,#3006,#3007));
#622=EDGE_LOOP('',(#3008));
#623=EDGE_LOOP('',(#3009));
#624=EDGE_LOOP('',(#3010,#3011,#3012,#3013));
#625=EDGE_LOOP('',(#3014));
#626=EDGE_LOOP('',(#3015,#3016,#3017,#3018));
#627=EDGE_LOOP('',(#3019,#3020,#3021,#3022));
#628=EDGE_LOOP('',(#3023,#3024,#3025,#3026));
#629=EDGE_LOOP('',(#3027));
#630=EDGE_LOOP('',(#3028,#3029,#3030,#3031));
#631=EDGE_LOOP('',(#3032,#3033,#3034,#3035));
#632=EDGE_LOOP('',(#3036,#3037,#3038,#3039));
#633=EDGE_LOOP('',(#3040,#3041,#3042,#3043));
#634=EDGE_LOOP('',(#3044,#3045,#3046,#3047));
#635=EDGE_LOOP('',(#3048,#3049,#3050,#3051));
#636=EDGE_LOOP('',(#3052,#3053,#3054,#3055));
#637=EDGE_LOOP('',(#3056,#3057,#3058,#3059));
#638=EDGE_LOOP('',(#3060,#3061,#3062,#3063));
#639=EDGE_LOOP('',(#3064,#3065,#3066,#3067));
#640=EDGE_LOOP('',(#3068,#3069,#3070,#3071));
#641=EDGE_LOOP('',(#3072,#3073,#3074,#3075));
#642=EDGE_LOOP('',(#3076,#3077,#3078,#3079));
#643=EDGE_LOOP('',(#3080,#3081,#3082,#3083));
#644=EDGE_LOOP('',(#3084,#3085,#3086,#3087,#3088,#3089,#3090,#3091,#3092,
#3093));
#645=EDGE_LOOP('',(#3094));
#646=EDGE_LOOP('',(#3095));
#647=EDGE_LOOP('',(#3096));
#648=EDGE_LOOP('',(#3097));
#649=EDGE_LOOP('',(#3098,#3099,#3100,#3101,#3102,#3103,#3104,#3105,#3106,
#3107));
#650=EDGE_LOOP('',(#3108));
#651=EDGE_LOOP('',(#3109));
#652=EDGE_LOOP('',(#3110));
#653=EDGE_LOOP('',(#3111));
#654=EDGE_LOOP('',(#3112,#3113,#3114,#3115));
#655=EDGE_LOOP('',(#3116,#3117,#3118,#3119));
#656=EDGE_LOOP('',(#3120,#3121,#3122,#3123));
#657=EDGE_LOOP('',(#3124,#3125,#3126,#3127));
#658=EDGE_LOOP('',(#3128,#3129,#3130,#3131));
#659=EDGE_LOOP('',(#3132,#3133,#3134,#3135));
#660=EDGE_LOOP('',(#3136,#3137,#3138,#3139));
#661=EDGE_LOOP('',(#3140,#3141,#3142,#3143));
#662=EDGE_LOOP('',(#3144,#3145,#3146,#3147));
#663=EDGE_LOOP('',(#3148,#3149,#3150,#3151));
#664=EDGE_LOOP('',(#3152,#3153,#3154,#3155));
#665=EDGE_LOOP('',(#3156,#3157,#3158,#3159));
#666=EDGE_LOOP('',(#3160,#3161,#3162,#3163));
#667=EDGE_LOOP('',(#3164,#3165,#3166,#3167));
#668=EDGE_LOOP('',(#3168,#3169,#3170,#3171,#3172,#3173,#3174,#3175,#3176,
#3177));
#669=EDGE_LOOP('',(#3178));
#670=EDGE_LOOP('',(#3179));
#671=EDGE_LOOP('',(#3180));
#672=EDGE_LOOP('',(#3181));
#673=EDGE_LOOP('',(#3182,#3183,#3184,#3185,#3186,#3187,#3188,#3189,#3190,
#3191));
#674=EDGE_LOOP('',(#3192));
#675=EDGE_LOOP('',(#3193));
#676=EDGE_LOOP('',(#3194));
#677=EDGE_LOOP('',(#3195));
#678=EDGE_LOOP('',(#3196,#3197,#3198,#3199));
#679=EDGE_LOOP('',(#3200,#3201,#3202,#3203));
#680=EDGE_LOOP('',(#3204,#3205,#3206,#3207));
#681=EDGE_LOOP('',(#3208,#3209,#3210,#3211));
#682=EDGE_LOOP('',(#3212,#3213,#3214,#3215));
#683=EDGE_LOOP('',(#3216,#3217,#3218,#3219));
#684=EDGE_LOOP('',(#3220,#3221,#3222,#3223));
#685=EDGE_LOOP('',(#3224,#3225,#3226,#3227));
#686=EDGE_LOOP('',(#3228,#3229,#3230,#3231));
#687=EDGE_LOOP('',(#3232,#3233,#3234,#3235));
#688=EDGE_LOOP('',(#3236,#3237,#3238,#3239));
#689=EDGE_LOOP('',(#3240,#3241,#3242,#3243));
#690=EDGE_LOOP('',(#3244,#3245,#3246,#3247));
#691=EDGE_LOOP('',(#3248,#3249,#3250,#3251));
#692=EDGE_LOOP('',(#3252,#3253,#3254,#3255,#3256,#3257,#3258,#3259,#3260,
#3261));
#693=EDGE_LOOP('',(#3262));
#694=EDGE_LOOP('',(#3263));
#695=EDGE_LOOP('',(#3264));
#696=EDGE_LOOP('',(#3265));
#697=EDGE_LOOP('',(#3266,#3267,#3268,#3269,#3270,#3271,#3272,#3273,#3274,
#3275));
#698=EDGE_LOOP('',(#3276));
#699=EDGE_LOOP('',(#3277));
#700=EDGE_LOOP('',(#3278));
#701=EDGE_LOOP('',(#3279));
#702=EDGE_LOOP('',(#3280,#3281,#3282,#3283));
#703=EDGE_LOOP('',(#3284,#3285,#3286,#3287));
#704=EDGE_LOOP('',(#3288,#3289,#3290,#3291));
#705=EDGE_LOOP('',(#3292,#3293,#3294,#3295));
#706=EDGE_LOOP('',(#3296,#3297,#3298,#3299));
#707=EDGE_LOOP('',(#3300,#3301,#3302,#3303));
#708=EDGE_LOOP('',(#3304,#3305,#3306,#3307));
#709=EDGE_LOOP('',(#3308,#3309,#3310,#3311));
#710=EDGE_LOOP('',(#3312,#3313,#3314,#3315));
#711=EDGE_LOOP('',(#3316,#3317,#3318,#3319));
#712=EDGE_LOOP('',(#3320,#3321,#3322,#3323));
#713=EDGE_LOOP('',(#3324,#3325,#3326,#3327));
#714=EDGE_LOOP('',(#3328,#3329,#3330,#3331));
#715=EDGE_LOOP('',(#3332,#3333,#3334,#3335));
#716=EDGE_LOOP('',(#3336,#3337,#3338,#3339,#3340,#3341,#3342,#3343,#3344,
#3345));
#717=EDGE_LOOP('',(#3346));
#718=EDGE_LOOP('',(#3347));
#719=EDGE_LOOP('',(#3348));
#720=EDGE_LOOP('',(#3349));
#721=EDGE_LOOP('',(#3350,#3351,#3352,#3353,#3354,#3355,#3356,#3357,#3358,
#3359));
#722=EDGE_LOOP('',(#3360));
#723=EDGE_LOOP('',(#3361));
#724=EDGE_LOOP('',(#3362));
#725=EDGE_LOOP('',(#3363));
#726=LINE('',#5062,#1105);
#727=LINE('',#5068,#1106);
#728=LINE('',#5073,#1107);
#729=LINE('',#5075,#1108);
#730=LINE('',#5077,#1109);
#731=LINE('',#5078,#1110);
#732=LINE('',#5084,#1111);
#733=LINE('',#5088,#1112);
#734=LINE('',#5089,#1113);
#735=LINE('',#5090,#1114);
#736=LINE('',#5094,#1115);
#737=LINE('',#5096,#1116);
#738=LINE('',#5098,#1117);
#739=LINE('',#5099,#1118);
#740=LINE('',#5105,#1119);
#741=LINE('',#5109,#1120);
#742=LINE('',#5110,#1121);
#743=LINE('',#5111,#1122);
#744=LINE('',#5115,#1123);
#745=LINE('',#5117,#1124);
#746=LINE('',#5119,#1125);
#747=LINE('',#5120,#1126);
#748=LINE('',#5126,#1127);
#749=LINE('',#5130,#1128);
#750=LINE('',#5131,#1129);
#751=LINE('',#5132,#1130);
#752=LINE('',#5134,#1131);
#753=LINE('',#5135,#1132);
#754=LINE('',#5137,#1133);
#755=LINE('',#5139,#1134);
#756=LINE('',#5141,#1135);
#757=LINE('',#5143,#1136);
#758=LINE('',#5144,#1137);
#759=LINE('',#5147,#1138);
#760=LINE('',#5148,#1139);
#761=LINE('',#5150,#1140);
#762=LINE('',#5152,#1141);
#763=LINE('',#5155,#1142);
#764=LINE('',#5156,#1143);
#765=LINE('',#5160,#1144);
#766=LINE('',#5162,#1145);
#767=LINE('',#5164,#1146);
#768=LINE('',#5165,#1147);
#769=LINE('',#5169,#1148);
#770=LINE('',#5171,#1149);
#771=LINE('',#5173,#1150);
#772=LINE('',#5174,#1151);
#773=LINE('',#5181,#1152);
#774=LINE('',#5183,#1153);
#775=LINE('',#5185,#1154);
#776=LINE('',#5186,#1155);
#777=LINE('',#5190,#1156);
#778=LINE('',#5192,#1157);
#779=LINE('',#5194,#1158);
#780=LINE('',#5195,#1159);
#781=LINE('',#5202,#1160);
#782=LINE('',#5204,#1161);
#783=LINE('',#5206,#1162);
#784=LINE('',#5207,#1163);
#785=LINE('',#5211,#1164);
#786=LINE('',#5213,#1165);
#787=LINE('',#5215,#1166);
#788=LINE('',#5216,#1167);
#789=LINE('',#5222,#1168);
#790=LINE('',#5224,#1169);
#791=LINE('',#5225,#1170);
#792=LINE('',#5227,#1171);
#793=LINE('',#5228,#1172);
#794=LINE('',#5231,#1173);
#795=LINE('',#5233,#1174);
#796=LINE('',#5234,#1175);
#797=LINE('',#5236,#1176);
#798=LINE('',#5237,#1177);
#799=LINE('',#5239,#1178);
#800=LINE('',#5240,#1179);
#801=LINE('',#5244,#1180);
#802=LINE('',#5246,#1181);
#803=LINE('',#5248,#1182);
#804=LINE('',#5249,#1183);
#805=LINE('',#5252,#1184);
#806=LINE('',#5254,#1185);
#807=LINE('',#5255,#1186);
#808=LINE('',#5258,#1187);
#809=LINE('',#5259,#1188);
#810=LINE('',#5262,#1189);
#811=LINE('',#5263,#1190);
#812=LINE('',#5265,#1191);
#813=LINE('',#5269,#1192);
#814=LINE('',#5271,#1193);
#815=LINE('',#5273,#1194);
#816=LINE('',#5274,#1195);
#817=LINE('',#5276,#1196);
#818=LINE('',#5278,#1197);
#819=LINE('',#5280,#1198);
#820=LINE('',#5281,#1199);
#821=LINE('',#5284,#1200);
#822=LINE('',#5285,#1201);
#823=LINE('',#5288,#1202);
#824=LINE('',#5289,#1203);
#825=LINE('',#5292,#1204);
#826=LINE('',#5293,#1205);
#827=LINE('',#5296,#1206);
#828=LINE('',#5297,#1207);
#829=LINE('',#5300,#1208);
#830=LINE('',#5301,#1209);
#831=LINE('',#5304,#1210);
#832=LINE('',#5305,#1211);
#833=LINE('',#5308,#1212);
#834=LINE('',#5309,#1213);
#835=LINE('',#5311,#1214);
#836=LINE('',#5324,#1215);
#837=LINE('',#5339,#1216);
#838=LINE('',#5345,#1217);
#839=LINE('',#5350,#1218);
#840=LINE('',#5352,#1219);
#841=LINE('',#5354,#1220);
#842=LINE('',#5355,#1221);
#843=LINE('',#5359,#1222);
#844=LINE('',#5361,#1223);
#845=LINE('',#5363,#1224);
#846=LINE('',#5364,#1225);
#847=LINE('',#5366,#1226);
#848=LINE('',#5367,#1227);
#849=LINE('',#5370,#1228);
#850=LINE('',#5372,#1229);
#851=LINE('',#5373,#1230);
#852=LINE('',#5376,#1231);
#853=LINE('',#5378,#1232);
#854=LINE('',#5379,#1233);
#855=LINE('',#5384,#1234);
#856=LINE('',#5391,#1235);
#857=LINE('',#5398,#1236);
#858=LINE('',#5403,#1237);
#859=LINE('',#5406,#1238);
#860=LINE('',#5408,#1239);
#861=LINE('',#5409,#1240);
#862=LINE('',#5410,#1241);
#863=LINE('',#5411,#1242);
#864=LINE('',#5414,#1243);
#865=LINE('',#5415,#1244);
#866=LINE('',#5416,#1245);
#867=LINE('',#5418,#1246);
#868=LINE('',#5419,#1247);
#869=LINE('',#5424,#1248);
#870=LINE('',#5426,#1249);
#871=LINE('',#5427,#1250);
#872=LINE('',#5430,#1251);
#873=LINE('',#5432,#1252);
#874=LINE('',#5433,#1253);
#875=LINE('',#5443,#1254);
#876=LINE('',#5447,#1255);
#877=LINE('',#5451,#1256);
#878=LINE('',#5455,#1257);
#879=LINE('',#5458,#1258);
#880=LINE('',#5460,#1259);
#881=LINE('',#5461,#1260);
#882=LINE('',#5464,#1261);
#883=LINE('',#5466,#1262);
#884=LINE('',#5467,#1263);
#885=LINE('',#5470,#1264);
#886=LINE('',#5472,#1265);
#887=LINE('',#5473,#1266);
#888=LINE('',#5477,#1267);
#889=LINE('',#5479,#1268);
#890=LINE('',#5481,#1269);
#891=LINE('',#5482,#1270);
#892=LINE('',#5484,#1271);
#893=LINE('',#5485,#1272);
#894=LINE('',#5489,#1273);
#895=LINE('',#5491,#1274);
#896=LINE('',#5492,#1275);
#897=LINE('',#5494,#1276);
#898=LINE('',#5496,#1277);
#899=LINE('',#5497,#1278);
#900=LINE('',#5500,#1279);
#901=LINE('',#5501,#1280);
#902=LINE('',#5504,#1281);
#903=LINE('',#5505,#1282);
#904=LINE('',#5508,#1283);
#905=LINE('',#5509,#1284);
#906=LINE('',#5512,#1285);
#907=LINE('',#5513,#1286);
#908=LINE('',#5516,#1287);
#909=LINE('',#5517,#1288);
#910=LINE('',#5519,#1289);
#911=LINE('',#5527,#1290);
#912=LINE('',#5530,#1291);
#913=LINE('',#5533,#1292);
#914=LINE('',#5537,#1293);
#915=LINE('',#5541,#1294);
#916=LINE('',#5544,#1295);
#917=LINE('',#5547,#1296);
#918=LINE('',#5548,#1297);
#919=LINE('',#5552,#1298);
#920=LINE('',#5557,#1299);
#921=LINE('',#5558,#1300);
#922=LINE('',#5561,#1301);
#923=LINE('',#5562,#1302);
#924=LINE('',#5566,#1303);
#925=LINE('',#5568,#1304);
#926=LINE('',#5570,#1305);
#927=LINE('',#5577,#1306);
#928=LINE('',#5584,#1307);
#929=LINE('',#5593,#1308);
#930=LINE('',#5598,#1309);
#931=LINE('',#5600,#1310);
#932=LINE('',#5602,#1311);
#933=LINE('',#5603,#1312);
#934=LINE('',#5606,#1313);
#935=LINE('',#5608,#1314);
#936=LINE('',#5609,#1315);
#937=LINE('',#5612,#1316);
#938=LINE('',#5614,#1317);
#939=LINE('',#5615,#1318);
#940=LINE('',#5617,#1319);
#941=LINE('',#5618,#1320);
#942=LINE('',#5622,#1321);
#943=LINE('',#5624,#1322);
#944=LINE('',#5626,#1323);
#945=LINE('',#5627,#1324);
#946=LINE('',#5630,#1325);
#947=LINE('',#5632,#1326);
#948=LINE('',#5633,#1327);
#949=LINE('',#5636,#1328);
#950=LINE('',#5638,#1329);
#951=LINE('',#5640,#1330);
#952=LINE('',#5642,#1331);
#953=LINE('',#5644,#1332);
#954=LINE('',#5645,#1333);
#955=LINE('',#5649,#1334);
#956=LINE('',#5650,#1335);
#957=LINE('',#5651,#1336);
#958=LINE('',#5654,#1337);
#959=LINE('',#5655,#1338);
#960=LINE('',#5658,#1339);
#961=LINE('',#5659,#1340);
#962=LINE('',#5662,#1341);
#963=LINE('',#5663,#1342);
#964=LINE('',#5665,#1343);
#965=LINE('',#5667,#1344);
#966=LINE('',#5679,#1345);
#967=LINE('',#5692,#1346);
#968=LINE('',#5709,#1347);
#969=LINE('',#5717,#1348);
#970=LINE('',#5723,#1349);
#971=LINE('',#5729,#1350);
#972=LINE('',#5735,#1351);
#973=LINE('',#5740,#1352);
#974=LINE('',#5742,#1353);
#975=LINE('',#5744,#1354);
#976=LINE('',#5745,#1355);
#977=LINE('',#5748,#1356);
#978=LINE('',#5750,#1357);
#979=LINE('',#5751,#1358);
#980=LINE('',#5754,#1359);
#981=LINE('',#5756,#1360);
#982=LINE('',#5757,#1361);
#983=LINE('',#5760,#1362);
#984=LINE('',#5762,#1363);
#985=LINE('',#5763,#1364);
#986=LINE('',#5766,#1365);
#987=LINE('',#5768,#1366);
#988=LINE('',#5769,#1367);
#989=LINE('',#5772,#1368);
#990=LINE('',#5774,#1369);
#991=LINE('',#5775,#1370);
#992=LINE('',#5778,#1371);
#993=LINE('',#5780,#1372);
#994=LINE('',#5781,#1373);
#995=LINE('',#5784,#1374);
#996=LINE('',#5786,#1375);
#997=LINE('',#5787,#1376);
#998=LINE('',#5790,#1377);
#999=LINE('',#5792,#1378);
#1000=LINE('',#5793,#1379);
#1001=LINE('',#5795,#1380);
#1002=LINE('',#5796,#1381);
#1003=LINE('',#5804,#1382);
#1004=LINE('',#5810,#1383);
#1005=LINE('',#5816,#1384);
#1006=LINE('',#5822,#1385);
#1007=LINE('',#5827,#1386);
#1008=LINE('',#5829,#1387);
#1009=LINE('',#5831,#1388);
#1010=LINE('',#5832,#1389);
#1011=LINE('',#5835,#1390);
#1012=LINE('',#5837,#1391);
#1013=LINE('',#5838,#1392);
#1014=LINE('',#5841,#1393);
#1015=LINE('',#5843,#1394);
#1016=LINE('',#5844,#1395);
#1017=LINE('',#5847,#1396);
#1018=LINE('',#5849,#1397);
#1019=LINE('',#5850,#1398);
#1020=LINE('',#5853,#1399);
#1021=LINE('',#5855,#1400);
#1022=LINE('',#5856,#1401);
#1023=LINE('',#5859,#1402);
#1024=LINE('',#5861,#1403);
#1025=LINE('',#5862,#1404);
#1026=LINE('',#5865,#1405);
#1027=LINE('',#5867,#1406);
#1028=LINE('',#5868,#1407);
#1029=LINE('',#5871,#1408);
#1030=LINE('',#5873,#1409);
#1031=LINE('',#5874,#1410);
#1032=LINE('',#5877,#1411);
#1033=LINE('',#5879,#1412);
#1034=LINE('',#5880,#1413);
#1035=LINE('',#5882,#1414);
#1036=LINE('',#5883,#1415);
#1037=LINE('',#5891,#1416);
#1038=LINE('',#5897,#1417);
#1039=LINE('',#5903,#1418);
#1040=LINE('',#5909,#1419);
#1041=LINE('',#5914,#1420);
#1042=LINE('',#5916,#1421);
#1043=LINE('',#5918,#1422);
#1044=LINE('',#5919,#1423);
#1045=LINE('',#5922,#1424);
#1046=LINE('',#5924,#1425);
#1047=LINE('',#5925,#1426);
#1048=LINE('',#5928,#1427);
#1049=LINE('',#5930,#1428);
#1050=LINE('',#5931,#1429);
#1051=LINE('',#5934,#1430);
#1052=LINE('',#5936,#1431);
#1053=LINE('',#5937,#1432);
#1054=LINE('',#5940,#1433);
#1055=LINE('',#5942,#1434);
#1056=LINE('',#5943,#1435);
#1057=LINE('',#5946,#1436);
#1058=LINE('',#5948,#1437);
#1059=LINE('',#5949,#1438);
#1060=LINE('',#5952,#1439);
#1061=LINE('',#5954,#1440);
#1062=LINE('',#5955,#1441);
#1063=LINE('',#5958,#1442);
#1064=LINE('',#5960,#1443);
#1065=LINE('',#5961,#1444);
#1066=LINE('',#5964,#1445);
#1067=LINE('',#5966,#1446);
#1068=LINE('',#5967,#1447);
#1069=LINE('',#5969,#1448);
#1070=LINE('',#5970,#1449);
#1071=LINE('',#5978,#1450);
#1072=LINE('',#5984,#1451);
#1073=LINE('',#5990,#1452);
#1074=LINE('',#5996,#1453);
#1075=LINE('',#6001,#1454);
#1076=LINE('',#6003,#1455);
#1077=LINE('',#6005,#1456);
#1078=LINE('',#6006,#1457);
#1079=LINE('',#6009,#1458);
#1080=LINE('',#6011,#1459);
#1081=LINE('',#6012,#1460);
#1082=LINE('',#6015,#1461);
#1083=LINE('',#6017,#1462);
#1084=LINE('',#6018,#1463);
#1085=LINE('',#6021,#1464);
#1086=LINE('',#6023,#1465);
#1087=LINE('',#6024,#1466);
#1088=LINE('',#6027,#1467);
#1089=LINE('',#6029,#1468);
#1090=LINE('',#6030,#1469);
#1091=LINE('',#6033,#1470);
#1092=LINE('',#6035,#1471);
#1093=LINE('',#6036,#1472);
#1094=LINE('',#6039,#1473);
#1095=LINE('',#6041,#1474);
#1096=LINE('',#6042,#1475);
#1097=LINE('',#6045,#1476);
#1098=LINE('',#6047,#1477);
#1099=LINE('',#6048,#1478);
#1100=LINE('',#6051,#1479);
#1101=LINE('',#6053,#1480);
#1102=LINE('',#6054,#1481);
#1103=LINE('',#6056,#1482);
#1104=LINE('',#6057,#1483);
#1105=VECTOR('',#4051,11.);
#1106=VECTOR('',#4058,11.);
#1107=VECTOR('',#4063,10.);
#1108=VECTOR('',#4064,10.);
#1109=VECTOR('',#4065,10.);
#1110=VECTOR('',#4066,10.);
#1111=VECTOR('',#4073,10.);
#1112=VECTOR('',#4076,10.);
#1113=VECTOR('',#4077,10.);
#1114=VECTOR('',#4078,10.);
#1115=VECTOR('',#4081,10.);
#1116=VECTOR('',#4082,10.);
#1117=VECTOR('',#4083,10.);
#1118=VECTOR('',#4084,10.);
#1119=VECTOR('',#4091,10.);
#1120=VECTOR('',#4094,10.);
#1121=VECTOR('',#4095,10.);
#1122=VECTOR('',#4096,10.);
#1123=VECTOR('',#4099,10.);
#1124=VECTOR('',#4100,10.);
#1125=VECTOR('',#4101,10.);
#1126=VECTOR('',#4102,10.);
#1127=VECTOR('',#4109,10.);
#1128=VECTOR('',#4112,10.);
#1129=VECTOR('',#4113,10.);
#1130=VECTOR('',#4114,10.);
#1131=VECTOR('',#4117,10.);
#1132=VECTOR('',#4118,10.);
#1133=VECTOR('',#4119,10.);
#1134=VECTOR('',#4120,10.);
#1135=VECTOR('',#4121,10.);
#1136=VECTOR('',#4122,10.);
#1137=VECTOR('',#4123,10.);
#1138=VECTOR('',#4126,10.);
#1139=VECTOR('',#4127,10.);
#1140=VECTOR('',#4130,10.);
#1141=VECTOR('',#4133,10.);
#1142=VECTOR('',#4136,10.);
#1143=VECTOR('',#4137,10.);
#1144=VECTOR('',#4140,10.);
#1145=VECTOR('',#4141,10.);
#1146=VECTOR('',#4142,10.);
#1147=VECTOR('',#4143,10.);
#1148=VECTOR('',#4146,10.);
#1149=VECTOR('',#4147,10.);
#1150=VECTOR('',#4148,10.);
#1151=VECTOR('',#4149,10.);
#1152=VECTOR('',#4158,10.);
#1153=VECTOR('',#4159,10.);
#1154=VECTOR('',#4160,10.);
#1155=VECTOR('',#4161,10.);
#1156=VECTOR('',#4164,10.);
#1157=VECTOR('',#4165,10.);
#1158=VECTOR('',#4166,10.);
#1159=VECTOR('',#4167,10.);
#1160=VECTOR('',#4176,10.);
#1161=VECTOR('',#4177,10.);
#1162=VECTOR('',#4178,10.);
#1163=VECTOR('',#4179,10.);
#1164=VECTOR('',#4182,10.);
#1165=VECTOR('',#4183,10.);
#1166=VECTOR('',#4184,10.);
#1167=VECTOR('',#4185,10.);
#1168=VECTOR('',#4194,10.);
#1169=VECTOR('',#4195,10.);
#1170=VECTOR('',#4196,10.);
#1171=VECTOR('',#4199,10.);
#1172=VECTOR('',#4200,10.);
#1173=VECTOR('',#4203,10.);
#1174=VECTOR('',#4204,10.);
#1175=VECTOR('',#4205,10.);
#1176=VECTOR('',#4208,10.);
#1177=VECTOR('',#4209,10.);
#1178=VECTOR('',#4212,10.);
#1179=VECTOR('',#4213,10.);
#1180=VECTOR('',#4216,10.);
#1181=VECTOR('',#4217,10.);
#1182=VECTOR('',#4218,10.);
#1183=VECTOR('',#4219,10.);
#1184=VECTOR('',#4222,10.);
#1185=VECTOR('',#4223,10.);
#1186=VECTOR('',#4224,10.);
#1187=VECTOR('',#4227,10.);
#1188=VECTOR('',#4228,10.);
#1189=VECTOR('',#4231,10.);
#1190=VECTOR('',#4232,10.);
#1191=VECTOR('',#4235,10.);
#1192=VECTOR('',#4238,10.);
#1193=VECTOR('',#4239,10.);
#1194=VECTOR('',#4240,10.);
#1195=VECTOR('',#4241,10.);
#1196=VECTOR('',#4242,10.);
#1197=VECTOR('',#4243,10.);
#1198=VECTOR('',#4244,10.);
#1199=VECTOR('',#4245,10.);
#1200=VECTOR('',#4248,10.);
#1201=VECTOR('',#4249,10.);
#1202=VECTOR('',#4252,10.);
#1203=VECTOR('',#4253,10.);
#1204=VECTOR('',#4256,10.);
#1205=VECTOR('',#4257,10.);
#1206=VECTOR('',#4260,10.);
#1207=VECTOR('',#4261,10.);
#1208=VECTOR('',#4264,10.);
#1209=VECTOR('',#4265,10.);
#1210=VECTOR('',#4268,10.);
#1211=VECTOR('',#4269,10.);
#1212=VECTOR('',#4272,10.);
#1213=VECTOR('',#4273,10.);
#1214=VECTOR('',#4276,10.);
#1215=VECTOR('',#4293,12.5);
#1216=VECTOR('',#4314,7.5);
#1217=VECTOR('',#4321,11.);
#1218=VECTOR('',#4326,10.);
#1219=VECTOR('',#4327,10.);
#1220=VECTOR('',#4328,10.);
#1221=VECTOR('',#4329,10.);
#1222=VECTOR('',#4332,10.);
#1223=VECTOR('',#4333,10.);
#1224=VECTOR('',#4334,10.);
#1225=VECTOR('',#4335,10.);
#1226=VECTOR('',#4338,10.);
#1227=VECTOR('',#4339,10.);
#1228=VECTOR('',#4342,10.);
#1229=VECTOR('',#4343,10.);
#1230=VECTOR('',#4344,10.);
#1231=VECTOR('',#4347,10.);
#1232=VECTOR('',#4348,10.);
#1233=VECTOR('',#4349,10.);
#1234=VECTOR('',#4354,10.);
#1235=VECTOR('',#4361,10.);
#1236=VECTOR('',#4368,10.);
#1237=VECTOR('',#4373,10.);
#1238=VECTOR('',#4376,10.);
#1239=VECTOR('',#4377,10.);
#1240=VECTOR('',#4378,10.);
#1241=VECTOR('',#4379,10.);
#1242=VECTOR('',#4380,10.);
#1243=VECTOR('',#4383,10.);
#1244=VECTOR('',#4384,10.);
#1245=VECTOR('',#4385,10.);
#1246=VECTOR('',#4386,10.);
#1247=VECTOR('',#4387,10.);
#1248=VECTOR('',#4394,10.);
#1249=VECTOR('',#4395,10.);
#1250=VECTOR('',#4396,10.);
#1251=VECTOR('',#4399,10.);
#1252=VECTOR('',#4400,10.);
#1253=VECTOR('',#4401,10.);
#1254=VECTOR('',#4414,10.);
#1255=VECTOR('',#4419,10.);
#1256=VECTOR('',#4424,10.);
#1257=VECTOR('',#4429,10.);
#1258=VECTOR('',#4432,10.);
#1259=VECTOR('',#4433,10.);
#1260=VECTOR('',#4434,10.);
#1261=VECTOR('',#4437,10.);
#1262=VECTOR('',#4438,10.);
#1263=VECTOR('',#4439,10.);
#1264=VECTOR('',#4442,10.);
#1265=VECTOR('',#4443,10.);
#1266=VECTOR('',#4444,10.);
#1267=VECTOR('',#4447,10.);
#1268=VECTOR('',#4448,10.);
#1269=VECTOR('',#4449,10.);
#1270=VECTOR('',#4450,10.);
#1271=VECTOR('',#4453,10.);
#1272=VECTOR('',#4454,10.);
#1273=VECTOR('',#4457,10.);
#1274=VECTOR('',#4458,10.);
#1275=VECTOR('',#4459,10.);
#1276=VECTOR('',#4460,10.);
#1277=VECTOR('',#4461,10.);
#1278=VECTOR('',#4462,10.);
#1279=VECTOR('',#4465,10.);
#1280=VECTOR('',#4466,10.);
#1281=VECTOR('',#4469,10.);
#1282=VECTOR('',#4470,10.);
#1283=VECTOR('',#4473,10.);
#1284=VECTOR('',#4474,10.);
#1285=VECTOR('',#4477,10.);
#1286=VECTOR('',#4478,10.);
#1287=VECTOR('',#4481,10.);
#1288=VECTOR('',#4482,10.);
#1289=VECTOR('',#4485,10.);
#1290=VECTOR('',#4494,10.);
#1291=VECTOR('',#4497,10.);
#1292=VECTOR('',#4500,10.);
#1293=VECTOR('',#4503,10.);
#1294=VECTOR('',#4506,10.);
#1295=VECTOR('',#4509,10.);
#1296=VECTOR('',#4512,10.);
#1297=VECTOR('',#4513,10.);
#1298=VECTOR('',#4518,10.);
#1299=VECTOR('',#4523,10.);
#1300=VECTOR('',#4524,10.);
#1301=VECTOR('',#4527,10.);
#1302=VECTOR('',#4528,10.);
#1303=VECTOR('',#4533,10.);
#1304=VECTOR('',#4536,10.);
#1305=VECTOR('',#4539,10.);
#1306=VECTOR('',#4548,7.5);
#1307=VECTOR('',#4557,11.);
#1308=VECTOR('',#4570,11.);
#1309=VECTOR('',#4575,10.);
#1310=VECTOR('',#4576,10.);
#1311=VECTOR('',#4577,10.);
#1312=VECTOR('',#4578,10.);
#1313=VECTOR('',#4581,10.);
#1314=VECTOR('',#4582,10.);
#1315=VECTOR('',#4583,10.);
#1316=VECTOR('',#4586,10.);
#1317=VECTOR('',#4587,10.);
#1318=VECTOR('',#4588,10.);
#1319=VECTOR('',#4591,10.);
#1320=VECTOR('',#4592,10.);
#1321=VECTOR('',#4595,10.);
#1322=VECTOR('',#4596,10.);
#1323=VECTOR('',#4597,10.);
#1324=VECTOR('',#4598,10.);
#1325=VECTOR('',#4601,10.);
#1326=VECTOR('',#4602,10.);
#1327=VECTOR('',#4603,10.);
#1328=VECTOR('',#4606,10.);
#1329=VECTOR('',#4607,10.);
#1330=VECTOR('',#4608,10.);
#1331=VECTOR('',#4609,10.);
#1332=VECTOR('',#4610,10.);
#1333=VECTOR('',#4611,10.);
#1334=VECTOR('',#4614,10.);
#1335=VECTOR('',#4615,10.);
#1336=VECTOR('',#4616,10.);
#1337=VECTOR('',#4619,10.);
#1338=VECTOR('',#4620,10.);
#1339=VECTOR('',#4623,10.);
#1340=VECTOR('',#4624,10.);
#1341=VECTOR('',#4627,10.);
#1342=VECTOR('',#4628,10.);
#1343=VECTOR('',#4631,10.);
#1344=VECTOR('',#4634,10.);
#1345=VECTOR('',#4651,31.837899857748);
#1346=VECTOR('',#4668,13.946575006305);
#1347=VECTOR('',#4693,36.8878705819456);
#1348=VECTOR('',#4704,1.99999999999999);
#1349=VECTOR('',#4711,1.99999999999999);
#1350=VECTOR('',#4718,1.99999999999999);
#1351=VECTOR('',#4725,1.99999999999999);
#1352=VECTOR('',#4730,10.);
#1353=VECTOR('',#4731,10.);
#1354=VECTOR('',#4732,10.);
#1355=VECTOR('',#4733,10.);
#1356=VECTOR('',#4736,10.);
#1357=VECTOR('',#4737,10.);
#1358=VECTOR('',#4738,10.);
#1359=VECTOR('',#4741,10.);
#1360=VECTOR('',#4742,10.);
#1361=VECTOR('',#4743,10.);
#1362=VECTOR('',#4746,10.);
#1363=VECTOR('',#4747,10.);
#1364=VECTOR('',#4748,10.);
#1365=VECTOR('',#4751,10.);
#1366=VECTOR('',#4752,10.);
#1367=VECTOR('',#4753,10.);
#1368=VECTOR('',#4756,10.);
#1369=VECTOR('',#4757,10.);
#1370=VECTOR('',#4758,10.);
#1371=VECTOR('',#4761,10.);
#1372=VECTOR('',#4762,10.);
#1373=VECTOR('',#4763,10.);
#1374=VECTOR('',#4766,10.);
#1375=VECTOR('',#4767,10.);
#1376=VECTOR('',#4768,10.);
#1377=VECTOR('',#4771,10.);
#1378=VECTOR('',#4772,10.);
#1379=VECTOR('',#4773,10.);
#1380=VECTOR('',#4776,10.);
#1381=VECTOR('',#4777,10.);
#1382=VECTOR('',#4788,1.99999999999999);
#1383=VECTOR('',#4795,1.99999999999999);
#1384=VECTOR('',#4802,1.99999999999999);
#1385=VECTOR('',#4809,1.99999999999999);
#1386=VECTOR('',#4814,10.);
#1387=VECTOR('',#4815,10.);
#1388=VECTOR('',#4816,10.);
#1389=VECTOR('',#4817,10.);
#1390=VECTOR('',#4820,10.);
#1391=VECTOR('',#4821,10.);
#1392=VECTOR('',#4822,10.);
#1393=VECTOR('',#4825,10.);
#1394=VECTOR('',#4826,10.);
#1395=VECTOR('',#4827,10.);
#1396=VECTOR('',#4830,10.);
#1397=VECTOR('',#4831,10.);
#1398=VECTOR('',#4832,10.);
#1399=VECTOR('',#4835,10.);
#1400=VECTOR('',#4836,10.);
#1401=VECTOR('',#4837,10.);
#1402=VECTOR('',#4840,10.);
#1403=VECTOR('',#4841,10.);
#1404=VECTOR('',#4842,10.);
#1405=VECTOR('',#4845,10.);
#1406=VECTOR('',#4846,10.);
#1407=VECTOR('',#4847,10.);
#1408=VECTOR('',#4850,10.);
#1409=VECTOR('',#4851,10.);
#1410=VECTOR('',#4852,10.);
#1411=VECTOR('',#4855,10.);
#1412=VECTOR('',#4856,10.);
#1413=VECTOR('',#4857,10.);
#1414=VECTOR('',#4860,10.);
#1415=VECTOR('',#4861,10.);
#1416=VECTOR('',#4872,1.99999999999999);
#1417=VECTOR('',#4879,1.99999999999999);
#1418=VECTOR('',#4886,1.99999999999999);
#1419=VECTOR('',#4893,1.99999999999999);
#1420=VECTOR('',#4898,10.);
#1421=VECTOR('',#4899,10.);
#1422=VECTOR('',#4900,10.);
#1423=VECTOR('',#4901,10.);
#1424=VECTOR('',#4904,10.);
#1425=VECTOR('',#4905,10.);
#1426=VECTOR('',#4906,10.);
#1427=VECTOR('',#4909,10.);
#1428=VECTOR('',#4910,10.);
#1429=VECTOR('',#4911,10.);
#1430=VECTOR('',#4914,10.);
#1431=VECTOR('',#4915,10.);
#1432=VECTOR('',#4916,10.);
#1433=VECTOR('',#4919,10.);
#1434=VECTOR('',#4920,10.);
#1435=VECTOR('',#4921,10.);
#1436=VECTOR('',#4924,10.);
#1437=VECTOR('',#4925,10.);
#1438=VECTOR('',#4926,10.);
#1439=VECTOR('',#4929,10.);
#1440=VECTOR('',#4930,10.);
#1441=VECTOR('',#4931,10.);
#1442=VECTOR('',#4934,10.);
#1443=VECTOR('',#4935,10.);
#1444=VECTOR('',#4936,10.);
#1445=VECTOR('',#4939,10.);
#1446=VECTOR('',#4940,10.);
#1447=VECTOR('',#4941,10.);
#1448=VECTOR('',#4944,10.);
#1449=VECTOR('',#4945,10.);
#1450=VECTOR('',#4956,1.99999999999999);
#1451=VECTOR('',#4963,1.99999999999999);
#1452=VECTOR('',#4970,1.99999999999999);
#1453=VECTOR('',#4977,1.99999999999999);
#1454=VECTOR('',#4982,10.);
#1455=VECTOR('',#4983,10.);
#1456=VECTOR('',#4984,10.);
#1457=VECTOR('',#4985,10.);
#1458=VECTOR('',#4988,10.);
#1459=VECTOR('',#4989,10.);
#1460=VECTOR('',#4990,10.);
#1461=VECTOR('',#4993,10.);
#1462=VECTOR('',#4994,10.);
#1463=VECTOR('',#4995,10.);
#1464=VECTOR('',#4998,10.);
#1465=VECTOR('',#4999,10.);
#1466=VECTOR('',#5000,10.);
#1467=VECTOR('',#5003,10.);
#1468=VECTOR('',#5004,10.);
#1469=VECTOR('',#5005,10.);
#1470=VECTOR('',#5008,10.);
#1471=VECTOR('',#5009,10.);
#1472=VECTOR('',#5010,10.);
#1473=VECTOR('',#5013,10.);
#1474=VECTOR('',#5014,10.);
#1475=VECTOR('',#5015,10.);
#1476=VECTOR('',#5018,10.);
#1477=VECTOR('',#5019,10.);
#1478=VECTOR('',#5020,10.);
#1479=VECTOR('',#5023,10.);
#1480=VECTOR('',#5024,10.);
#1481=VECTOR('',#5025,10.);
#1482=VECTOR('',#5028,10.);
#1483=VECTOR('',#5029,10.);
#1484=CIRCLE('',#3729,11.);
#1485=CIRCLE('',#3730,11.);
#1486=CIRCLE('',#3732,11.);
#1487=CIRCLE('',#3733,11.);
#1488=CIRCLE('',#3736,7.61489399011346);
#1489=CIRCLE('',#3737,7.61489399011346);
#1490=CIRCLE('',#3741,7.61489399011346);
#1491=CIRCLE('',#3742,7.61489399011346);
#1492=CIRCLE('',#3746,7.61489399011346);
#1493=CIRCLE('',#3747,7.61489399011346);
#1494=CIRCLE('',#3757,7.61489399011346);
#1495=CIRCLE('',#3758,7.61489399011346);
#1496=CIRCLE('',#3762,7.61489399011346);
#1497=CIRCLE('',#3763,7.61489399011346);
#1498=CIRCLE('',#3767,7.61489399011346);
#1499=CIRCLE('',#3768,7.61489399011346);
#1500=CIRCLE('',#3791,12.);
#1501=CIRCLE('',#3792,0.5);
#1502=CIRCLE('',#3793,12.5);
#1503=CIRCLE('',#3794,12.5);
#1504=CIRCLE('',#3796,12.5);
#1505=CIRCLE('',#3797,12.5);
#1506=CIRCLE('',#3799,7.5);
#1507=CIRCLE('',#3801,0.5);
#1508=CIRCLE('',#3802,12.);
#1509=CIRCLE('',#3804,7.5);
#1510=CIRCLE('',#3808,11.5112);
#1511=CIRCLE('',#3809,11.5112);
#1512=CIRCLE('',#3816,10.);
#1513=CIRCLE('',#3818,10.);
#1514=CIRCLE('',#3819,10.);
#1515=CIRCLE('',#3821,10.);
#1516=CIRCLE('',#3822,10.);
#1517=CIRCLE('',#3824,10.);
#1518=CIRCLE('',#3828,10.);
#1519=CIRCLE('',#3829,10.);
#1520=CIRCLE('',#3831,10.);
#1521=CIRCLE('',#3832,10.);
#1522=CIRCLE('',#3833,10.);
#1523=CIRCLE('',#3834,10.);
#1524=CIRCLE('',#3836,10.);
#1525=CIRCLE('',#3838,10.);
#1526=CIRCLE('',#3840,10.);
#1527=CIRCLE('',#3842,10.);
#1528=CIRCLE('',#3858,5.);
#1529=CIRCLE('',#3859,5.);
#1530=CIRCLE('',#3861,5.);
#1531=CIRCLE('',#3862,5.);
#1532=CIRCLE('',#3863,5.);
#1533=CIRCLE('',#3866,5.);
#1534=CIRCLE('',#3868,5.);
#1535=CIRCLE('',#3871,5.);
#1536=CIRCLE('',#3877,7.5);
#1537=CIRCLE('',#3878,7.5);
#1538=CIRCLE('',#3881,10.88225);
#1539=CIRCLE('',#3882,10.88225);
#1540=CIRCLE('',#3887,11.);
#1541=CIRCLE('',#3888,11.);
#1542=CIRCLE('',#3905,33.837899857748);
#1543=CIRCLE('',#3906,2.);
#1544=CIRCLE('',#3907,31.837899857748);
#1545=CIRCLE('',#3909,31.837899857748);
#1546=CIRCLE('',#3911,34.8878705819456);
#1547=CIRCLE('',#3913,15.946575006305);
#1548=CIRCLE('',#3914,2.);
#1549=CIRCLE('',#3915,13.946575006305);
#1550=CIRCLE('',#3917,13.946575006305);
#1551=CIRCLE('',#3919,29.837899857748);
#1552=CIRCLE('',#3921,11.946575006305);
#1553=CIRCLE('',#3922,2.);
#1554=CIRCLE('',#3925,2.);
#1555=CIRCLE('',#3927,2.);
#1556=CIRCLE('',#3928,36.8878705819456);
#1557=CIRCLE('',#3930,36.8878705819456);
#1558=CIRCLE('',#3934,1.99999999999999);
#1559=CIRCLE('',#3935,1.99999999999999);
#1560=CIRCLE('',#3937,1.99999999999999);
#1561=CIRCLE('',#3938,1.99999999999999);
#1562=CIRCLE('',#3940,1.99999999999999);
#1563=CIRCLE('',#3941,1.99999999999999);
#1564=CIRCLE('',#3943,1.99999999999999);
#1565=CIRCLE('',#3944,1.99999999999999);
#1566=CIRCLE('',#3959,1.99999999999999);
#1567=CIRCLE('',#3960,1.99999999999999);
#1568=CIRCLE('',#3962,1.99999999999999);
#1569=CIRCLE('',#3963,1.99999999999999);
#1570=CIRCLE('',#3965,1.99999999999999);
#1571=CIRCLE('',#3966,1.99999999999999);
#1572=CIRCLE('',#3968,1.99999999999999);
#1573=CIRCLE('',#3969,1.99999999999999);
#1574=CIRCLE('',#3984,1.99999999999999);
#1575=CIRCLE('',#3985,1.99999999999999);
#1576=CIRCLE('',#3987,1.99999999999999);
#1577=CIRCLE('',#3988,1.99999999999999);
#1578=CIRCLE('',#3990,1.99999999999999);
#1579=CIRCLE('',#3991,1.99999999999999);
#1580=CIRCLE('',#3993,1.99999999999999);
#1581=CIRCLE('',#3994,1.99999999999999);
#1582=CIRCLE('',#4009,1.99999999999999);
#1583=CIRCLE('',#4010,1.99999999999999);
#1584=CIRCLE('',#4012,1.99999999999999);
#1585=CIRCLE('',#4013,1.99999999999999);
#1586=CIRCLE('',#4015,1.99999999999999);
#1587=CIRCLE('',#4016,1.99999999999999);
#1588=CIRCLE('',#4018,1.99999999999999);
#1589=CIRCLE('',#4019,1.99999999999999);
#1590=VERTEX_POINT('',#5059);
#1591=VERTEX_POINT('',#5061);
#1592=VERTEX_POINT('',#5065);
#1593=VERTEX_POINT('',#5067);
#1594=VERTEX_POINT('',#5071);
#1595=VERTEX_POINT('',#5072);
#1596=VERTEX_POINT('',#5074);
#1597=VERTEX_POINT('',#5076);
#1598=VERTEX_POINT('',#5080);
#1599=VERTEX_POINT('',#5082);
#1600=VERTEX_POINT('',#5086);
#1601=VERTEX_POINT('',#5087);
#1602=VERTEX_POINT('',#5092);
#1603=VERTEX_POINT('',#5093);
#1604=VERTEX_POINT('',#5095);
#1605=VERTEX_POINT('',#5097);
#1606=VERTEX_POINT('',#5101);
#1607=VERTEX_POINT('',#5103);
#1608=VERTEX_POINT('',#5107);
#1609=VERTEX_POINT('',#5108);
#1610=VERTEX_POINT('',#5113);
#1611=VERTEX_POINT('',#5114);
#1612=VERTEX_POINT('',#5116);
#1613=VERTEX_POINT('',#5118);
#1614=VERTEX_POINT('',#5122);
#1615=VERTEX_POINT('',#5124);
#1616=VERTEX_POINT('',#5128);
#1617=VERTEX_POINT('',#5129);
#1618=VERTEX_POINT('',#5136);
#1619=VERTEX_POINT('',#5138);
#1620=VERTEX_POINT('',#5140);
#1621=VERTEX_POINT('',#5142);
#1622=VERTEX_POINT('',#5146);
#1623=VERTEX_POINT('',#5154);
#1624=VERTEX_POINT('',#5158);
#1625=VERTEX_POINT('',#5159);
#1626=VERTEX_POINT('',#5161);
#1627=VERTEX_POINT('',#5163);
#1628=VERTEX_POINT('',#5167);
#1629=VERTEX_POINT('',#5168);
#1630=VERTEX_POINT('',#5170);
#1631=VERTEX_POINT('',#5172);
#1632=VERTEX_POINT('',#5179);
#1633=VERTEX_POINT('',#5180);
#1634=VERTEX_POINT('',#5182);
#1635=VERTEX_POINT('',#5184);
#1636=VERTEX_POINT('',#5188);
#1637=VERTEX_POINT('',#5189);
#1638=VERTEX_POINT('',#5191);
#1639=VERTEX_POINT('',#5193);
#1640=VERTEX_POINT('',#5200);
#1641=VERTEX_POINT('',#5201);
#1642=VERTEX_POINT('',#5203);
#1643=VERTEX_POINT('',#5205);
#1644=VERTEX_POINT('',#5209);
#1645=VERTEX_POINT('',#5210);
#1646=VERTEX_POINT('',#5212);
#1647=VERTEX_POINT('',#5214);
#1648=VERTEX_POINT('',#5221);
#1649=VERTEX_POINT('',#5223);
#1650=VERTEX_POINT('',#5230);
#1651=VERTEX_POINT('',#5232);
#1652=VERTEX_POINT('',#5242);
#1653=VERTEX_POINT('',#5243);
#1654=VERTEX_POINT('',#5245);
#1655=VERTEX_POINT('',#5247);
#1656=VERTEX_POINT('',#5251);
#1657=VERTEX_POINT('',#5253);
#1658=VERTEX_POINT('',#5257);
#1659=VERTEX_POINT('',#5261);
#1660=VERTEX_POINT('',#5267);
#1661=VERTEX_POINT('',#5268);
#1662=VERTEX_POINT('',#5270);
#1663=VERTEX_POINT('',#5272);
#1664=VERTEX_POINT('',#5275);
#1665=VERTEX_POINT('',#5277);
#1666=VERTEX_POINT('',#5279);
#1667=VERTEX_POINT('',#5283);
#1668=VERTEX_POINT('',#5287);
#1669=VERTEX_POINT('',#5291);
#1670=VERTEX_POINT('',#5295);
#1671=VERTEX_POINT('',#5299);
#1672=VERTEX_POINT('',#5303);
#1673=VERTEX_POINT('',#5307);
#1674=VERTEX_POINT('',#5315);
#1675=VERTEX_POINT('',#5317);
#1676=VERTEX_POINT('',#5319);
#1677=VERTEX_POINT('',#5323);
#1678=VERTEX_POINT('',#5325);
#1679=VERTEX_POINT('',#5329);
#1680=VERTEX_POINT('',#5332);
#1681=VERTEX_POINT('',#5336);
#1682=VERTEX_POINT('',#5342);
#1683=VERTEX_POINT('',#5344);
#1684=VERTEX_POINT('',#5348);
#1685=VERTEX_POINT('',#5349);
#1686=VERTEX_POINT('',#5351);
#1687=VERTEX_POINT('',#5353);
#1688=VERTEX_POINT('',#5357);
#1689=VERTEX_POINT('',#5358);
#1690=VERTEX_POINT('',#5360);
#1691=VERTEX_POINT('',#5362);
#1692=VERTEX_POINT('',#5369);
#1693=VERTEX_POINT('',#5371);
#1694=VERTEX_POINT('',#5375);
#1695=VERTEX_POINT('',#5377);
#1696=VERTEX_POINT('',#5381);
#1697=VERTEX_POINT('',#5382);
#1698=VERTEX_POINT('',#5386);
#1699=VERTEX_POINT('',#5387);
#1700=VERTEX_POINT('',#5389);
#1701=VERTEX_POINT('',#5393);
#1702=VERTEX_POINT('',#5394);
#1703=VERTEX_POINT('',#5396);
#1704=VERTEX_POINT('',#5400);
#1705=VERTEX_POINT('',#5401);
#1706=VERTEX_POINT('',#5405);
#1707=VERTEX_POINT('',#5407);
#1708=VERTEX_POINT('',#5413);
#1709=VERTEX_POINT('',#5417);
#1710=VERTEX_POINT('',#5423);
#1711=VERTEX_POINT('',#5425);
#1712=VERTEX_POINT('',#5429);
#1713=VERTEX_POINT('',#5431);
#1714=VERTEX_POINT('',#5434);
#1715=VERTEX_POINT('',#5437);
#1716=VERTEX_POINT('',#5441);
#1717=VERTEX_POINT('',#5445);
#1718=VERTEX_POINT('',#5449);
#1719=VERTEX_POINT('',#5453);
#1720=VERTEX_POINT('',#5457);
#1721=VERTEX_POINT('',#5459);
#1722=VERTEX_POINT('',#5463);
#1723=VERTEX_POINT('',#5465);
#1724=VERTEX_POINT('',#5469);
#1725=VERTEX_POINT('',#5471);
#1726=VERTEX_POINT('',#5475);
#1727=VERTEX_POINT('',#5476);
#1728=VERTEX_POINT('',#5478);
#1729=VERTEX_POINT('',#5480);
#1730=VERTEX_POINT('',#5487);
#1731=VERTEX_POINT('',#5488);
#1732=VERTEX_POINT('',#5490);
#1733=VERTEX_POINT('',#5493);
#1734=VERTEX_POINT('',#5495);
#1735=VERTEX_POINT('',#5499);
#1736=VERTEX_POINT('',#5503);
#1737=VERTEX_POINT('',#5507);
#1738=VERTEX_POINT('',#5511);
#1739=VERTEX_POINT('',#5515);
#1740=VERTEX_POINT('',#5523);
#1741=VERTEX_POINT('',#5524);
#1742=VERTEX_POINT('',#5526);
#1743=VERTEX_POINT('',#5528);
#1744=VERTEX_POINT('',#5532);
#1745=VERTEX_POINT('',#5534);
#1746=VERTEX_POINT('',#5536);
#1747=VERTEX_POINT('',#5538);
#1748=VERTEX_POINT('',#5540);
#1749=VERTEX_POINT('',#5542);
#1750=VERTEX_POINT('',#5546);
#1751=VERTEX_POINT('',#5550);
#1752=VERTEX_POINT('',#5554);
#1753=VERTEX_POINT('',#5555);
#1754=VERTEX_POINT('',#5560);
#1755=VERTEX_POINT('',#5564);
#1756=VERTEX_POINT('',#5574);
#1757=VERTEX_POINT('',#5576);
#1758=VERTEX_POINT('',#5581);
#1759=VERTEX_POINT('',#5583);
#1760=VERTEX_POINT('',#5590);
#1761=VERTEX_POINT('',#5592);
#1762=VERTEX_POINT('',#5596);
#1763=VERTEX_POINT('',#5597);
#1764=VERTEX_POINT('',#5599);
#1765=VERTEX_POINT('',#5601);
#1766=VERTEX_POINT('',#5605);
#1767=VERTEX_POINT('',#5607);
#1768=VERTEX_POINT('',#5611);
#1769=VERTEX_POINT('',#5613);
#1770=VERTEX_POINT('',#5620);
#1771=VERTEX_POINT('',#5621);
#1772=VERTEX_POINT('',#5623);
#1773=VERTEX_POINT('',#5625);
#1774=VERTEX_POINT('',#5629);
#1775=VERTEX_POINT('',#5631);
#1776=VERTEX_POINT('',#5635);
#1777=VERTEX_POINT('',#5637);
#1778=VERTEX_POINT('',#5639);
#1779=VERTEX_POINT('',#5641);
#1780=VERTEX_POINT('',#5643);
#1781=VERTEX_POINT('',#5647);
#1782=VERTEX_POINT('',#5648);
#1783=VERTEX_POINT('',#5653);
#1784=VERTEX_POINT('',#5657);
#1785=VERTEX_POINT('',#5661);
#1786=VERTEX_POINT('',#5671);
#1787=VERTEX_POINT('',#5673);
#1788=VERTEX_POINT('',#5677);
#1789=VERTEX_POINT('',#5681);
#1790=VERTEX_POINT('',#5684);
#1791=VERTEX_POINT('',#5686);
#1792=VERTEX_POINT('',#5690);
#1793=VERTEX_POINT('',#5694);
#1794=VERTEX_POINT('',#5697);
#1795=VERTEX_POINT('',#5704);
#1796=VERTEX_POINT('',#5708);
#1797=VERTEX_POINT('',#5714);
#1798=VERTEX_POINT('',#5716);
#1799=VERTEX_POINT('',#5720);
#1800=VERTEX_POINT('',#5722);
#1801=VERTEX_POINT('',#5726);
#1802=VERTEX_POINT('',#5728);
#1803=VERTEX_POINT('',#5732);
#1804=VERTEX_POINT('',#5734);
#1805=VERTEX_POINT('',#5738);
#1806=VERTEX_POINT('',#5739);
#1807=VERTEX_POINT('',#5741);
#1808=VERTEX_POINT('',#5743);
#1809=VERTEX_POINT('',#5747);
#1810=VERTEX_POINT('',#5749);
#1811=VERTEX_POINT('',#5753);
#1812=VERTEX_POINT('',#5755);
#1813=VERTEX_POINT('',#5759);
#1814=VERTEX_POINT('',#5761);
#1815=VERTEX_POINT('',#5765);
#1816=VERTEX_POINT('',#5767);
#1817=VERTEX_POINT('',#5771);
#1818=VERTEX_POINT('',#5773);
#1819=VERTEX_POINT('',#5777);
#1820=VERTEX_POINT('',#5779);
#1821=VERTEX_POINT('',#5783);
#1822=VERTEX_POINT('',#5785);
#1823=VERTEX_POINT('',#5789);
#1824=VERTEX_POINT('',#5791);
#1825=VERTEX_POINT('',#5801);
#1826=VERTEX_POINT('',#5803);
#1827=VERTEX_POINT('',#5807);
#1828=VERTEX_POINT('',#5809);
#1829=VERTEX_POINT('',#5813);
#1830=VERTEX_POINT('',#5815);
#1831=VERTEX_POINT('',#5819);
#1832=VERTEX_POINT('',#5821);
#1833=VERTEX_POINT('',#5825);
#1834=VERTEX_POINT('',#5826);
#1835=VERTEX_POINT('',#5828);
#1836=VERTEX_POINT('',#5830);
#1837=VERTEX_POINT('',#5834);
#1838=VERTEX_POINT('',#5836);
#1839=VERTEX_POINT('',#5840);
#1840=VERTEX_POINT('',#5842);
#1841=VERTEX_POINT('',#5846);
#1842=VERTEX_POINT('',#5848);
#1843=VERTEX_POINT('',#5852);
#1844=VERTEX_POINT('',#5854);
#1845=VERTEX_POINT('',#5858);
#1846=VERTEX_POINT('',#5860);
#1847=VERTEX_POINT('',#5864);
#1848=VERTEX_POINT('',#5866);
#1849=VERTEX_POINT('',#5870);
#1850=VERTEX_POINT('',#5872);
#1851=VERTEX_POINT('',#5876);
#1852=VERTEX_POINT('',#5878);
#1853=VERTEX_POINT('',#5888);
#1854=VERTEX_POINT('',#5890);
#1855=VERTEX_POINT('',#5894);
#1856=VERTEX_POINT('',#5896);
#1857=VERTEX_POINT('',#5900);
#1858=VERTEX_POINT('',#5902);
#1859=VERTEX_POINT('',#5906);
#1860=VERTEX_POINT('',#5908);
#1861=VERTEX_POINT('',#5912);
#1862=VERTEX_POINT('',#5913);
#1863=VERTEX_POINT('',#5915);
#1864=VERTEX_POINT('',#5917);
#1865=VERTEX_POINT('',#5921);
#1866=VERTEX_POINT('',#5923);
#1867=VERTEX_POINT('',#5927);
#1868=VERTEX_POINT('',#5929);
#1869=VERTEX_POINT('',#5933);
#1870=VERTEX_POINT('',#5935);
#1871=VERTEX_POINT('',#5939);
#1872=VERTEX_POINT('',#5941);
#1873=VERTEX_POINT('',#5945);
#1874=VERTEX_POINT('',#5947);
#1875=VERTEX_POINT('',#5951);
#1876=VERTEX_POINT('',#5953);
#1877=VERTEX_POINT('',#5957);
#1878=VERTEX_POINT('',#5959);
#1879=VERTEX_POINT('',#5963);
#1880=VERTEX_POINT('',#5965);
#1881=VERTEX_POINT('',#5975);
#1882=VERTEX_POINT('',#5977);
#1883=VERTEX_POINT('',#5981);
#1884=VERTEX_POINT('',#5983);
#1885=VERTEX_POINT('',#5987);
#1886=VERTEX_POINT('',#5989);
#1887=VERTEX_POINT('',#5993);
#1888=VERTEX_POINT('',#5995);
#1889=VERTEX_POINT('',#5999);
#1890=VERTEX_POINT('',#6000);
#1891=VERTEX_POINT('',#6002);
#1892=VERTEX_POINT('',#6004);
#1893=VERTEX_POINT('',#6008);
#1894=VERTEX_POINT('',#6010);
#1895=VERTEX_POINT('',#6014);
#1896=VERTEX_POINT('',#6016);
#1897=VERTEX_POINT('',#6020);
#1898=VERTEX_POINT('',#6022);
#1899=VERTEX_POINT('',#6026);
#1900=VERTEX_POINT('',#6028);
#1901=VERTEX_POINT('',#6032);
#1902=VERTEX_POINT('',#6034);
#1903=VERTEX_POINT('',#6038);
#1904=VERTEX_POINT('',#6040);
#1905=VERTEX_POINT('',#6044);
#1906=VERTEX_POINT('',#6046);
#1907=VERTEX_POINT('',#6050);
#1908=VERTEX_POINT('',#6052);
#1909=EDGE_CURVE('',#1590,#1590,#1484,.T.);
#1910=EDGE_CURVE('',#1590,#1591,#726,.T.);
#1911=EDGE_CURVE('',#1591,#1591,#1485,.T.);
#1912=EDGE_CURVE('',#1592,#1592,#1486,.T.);
#1913=EDGE_CURVE('',#1592,#1593,#727,.T.);
#1914=EDGE_CURVE('',#1593,#1593,#1487,.T.);
#1915=EDGE_CURVE('',#1594,#1595,#728,.T.);
#1916=EDGE_CURVE('',#1596,#1594,#729,.T.);
#1917=EDGE_CURVE('',#1596,#1597,#730,.T.);
#1918=EDGE_CURVE('',#1595,#1597,#731,.T.);
#1919=EDGE_CURVE('',#1597,#1598,#1488,.T.);
#1920=EDGE_CURVE('',#1599,#1596,#1489,.T.);
#1921=EDGE_CURVE('',#1599,#1598,#732,.T.);
#1922=EDGE_CURVE('',#1600,#1601,#733,.T.);
#1923=EDGE_CURVE('',#1598,#1600,#734,.T.);
#1924=EDGE_CURVE('',#1601,#1599,#735,.T.);
#1925=EDGE_CURVE('',#1602,#1603,#736,.T.);
#1926=EDGE_CURVE('',#1604,#1602,#737,.T.);
#1927=EDGE_CURVE('',#1604,#1605,#738,.T.);
#1928=EDGE_CURVE('',#1603,#1605,#739,.T.);
#1929=EDGE_CURVE('',#1605,#1606,#1490,.T.);
#1930=EDGE_CURVE('',#1607,#1604,#1491,.T.);
#1931=EDGE_CURVE('',#1607,#1606,#740,.T.);
#1932=EDGE_CURVE('',#1608,#1609,#741,.T.);
#1933=EDGE_CURVE('',#1606,#1608,#742,.T.);
#1934=EDGE_CURVE('',#1609,#1607,#743,.T.);
#1935=EDGE_CURVE('',#1610,#1611,#744,.T.);
#1936=EDGE_CURVE('',#1612,#1610,#745,.T.);
#1937=EDGE_CURVE('',#1612,#1613,#746,.T.);
#1938=EDGE_CURVE('',#1611,#1613,#747,.T.);
#1939=EDGE_CURVE('',#1613,#1614,#1492,.T.);
#1940=EDGE_CURVE('',#1615,#1612,#1493,.T.);
#1941=EDGE_CURVE('',#1615,#1614,#748,.T.);
#1942=EDGE_CURVE('',#1616,#1617,#749,.T.);
#1943=EDGE_CURVE('',#1614,#1616,#750,.T.);
#1944=EDGE_CURVE('',#1617,#1615,#751,.T.);
#1945=EDGE_CURVE('',#1611,#1600,#752,.T.);
#1946=EDGE_CURVE('',#1603,#1616,#753,.T.);
#1947=EDGE_CURVE('',#1618,#1608,#754,.T.);
#1948=EDGE_CURVE('',#1618,#1619,#755,.T.);
#1949=EDGE_CURVE('',#1619,#1620,#756,.T.);
#1950=EDGE_CURVE('',#1621,#1620,#757,.T.);
#1951=EDGE_CURVE('',#1595,#1621,#758,.T.);
#1952=EDGE_CURVE('',#1622,#1609,#759,.T.);
#1953=EDGE_CURVE('',#1622,#1618,#760,.T.);
#1954=EDGE_CURVE('',#1602,#1617,#761,.T.);
#1955=EDGE_CURVE('',#1610,#1601,#762,.T.);
#1956=EDGE_CURVE('',#1623,#1621,#763,.T.);
#1957=EDGE_CURVE('',#1594,#1623,#764,.T.);
#1958=EDGE_CURVE('',#1624,#1625,#765,.T.);
#1959=EDGE_CURVE('',#1626,#1624,#766,.T.);
#1960=EDGE_CURVE('',#1627,#1626,#767,.T.);
#1961=EDGE_CURVE('',#1625,#1627,#768,.T.);
#1962=EDGE_CURVE('',#1628,#1629,#769,.T.);
#1963=EDGE_CURVE('',#1630,#1628,#770,.T.);
#1964=EDGE_CURVE('',#1631,#1630,#771,.T.);
#1965=EDGE_CURVE('',#1631,#1629,#772,.T.);
#1966=EDGE_CURVE('',#1629,#1624,#1494,.T.);
#1967=EDGE_CURVE('',#1626,#1631,#1495,.T.);
#1968=EDGE_CURVE('',#1632,#1633,#773,.T.);
#1969=EDGE_CURVE('',#1634,#1632,#774,.T.);
#1970=EDGE_CURVE('',#1635,#1634,#775,.T.);
#1971=EDGE_CURVE('',#1633,#1635,#776,.T.);
#1972=EDGE_CURVE('',#1636,#1637,#777,.T.);
#1973=EDGE_CURVE('',#1638,#1636,#778,.T.);
#1974=EDGE_CURVE('',#1639,#1638,#779,.T.);
#1975=EDGE_CURVE('',#1639,#1637,#780,.T.);
#1976=EDGE_CURVE('',#1637,#1632,#1496,.T.);
#1977=EDGE_CURVE('',#1634,#1639,#1497,.T.);
#1978=EDGE_CURVE('',#1640,#1641,#781,.T.);
#1979=EDGE_CURVE('',#1642,#1640,#782,.T.);
#1980=EDGE_CURVE('',#1643,#1642,#783,.T.);
#1981=EDGE_CURVE('',#1641,#1643,#784,.T.);
#1982=EDGE_CURVE('',#1644,#1645,#785,.T.);
#1983=EDGE_CURVE('',#1646,#1644,#786,.T.);
#1984=EDGE_CURVE('',#1647,#1646,#787,.T.);
#1985=EDGE_CURVE('',#1647,#1645,#788,.T.);
#1986=EDGE_CURVE('',#1645,#1640,#1498,.T.);
#1987=EDGE_CURVE('',#1642,#1647,#1499,.T.);
#1988=EDGE_CURVE('',#1643,#1648,#789,.T.);
#1989=EDGE_CURVE('',#1649,#1648,#790,.T.);
#1990=EDGE_CURVE('',#1641,#1649,#791,.T.);
#1991=EDGE_CURVE('',#1635,#1646,#792,.T.);
#1992=EDGE_CURVE('',#1633,#1644,#793,.T.);
#1993=EDGE_CURVE('',#1650,#1628,#794,.T.);
#1994=EDGE_CURVE('',#1650,#1651,#795,.T.);
#1995=EDGE_CURVE('',#1651,#1630,#796,.T.);
#1996=EDGE_CURVE('',#1627,#1638,#797,.T.);
#1997=EDGE_CURVE('',#1625,#1636,#798,.T.);
#1998=EDGE_CURVE('',#1648,#1623,#799,.T.);
#1999=EDGE_CURVE('',#1651,#1622,#800,.T.);
#2000=EDGE_CURVE('',#1652,#1653,#801,.T.);
#2001=EDGE_CURVE('',#1654,#1652,#802,.T.);
#2002=EDGE_CURVE('',#1655,#1654,#803,.T.);
#2003=EDGE_CURVE('',#1653,#1655,#804,.T.);
#2004=EDGE_CURVE('',#1656,#1655,#805,.T.);
#2005=EDGE_CURVE('',#1656,#1657,#806,.T.);
#2006=EDGE_CURVE('',#1657,#1653,#807,.T.);
#2007=EDGE_CURVE('',#1658,#1654,#808,.T.);
#2008=EDGE_CURVE('',#1658,#1656,#809,.T.);
#2009=EDGE_CURVE('',#1659,#1652,#810,.T.);
#2010=EDGE_CURVE('',#1659,#1658,#811,.T.);
#2011=EDGE_CURVE('',#1659,#1657,#812,.T.);
#2012=EDGE_CURVE('',#1660,#1661,#813,.T.);
#2013=EDGE_CURVE('',#1662,#1660,#814,.T.);
#2014=EDGE_CURVE('',#1663,#1662,#815,.T.);
#2015=EDGE_CURVE('',#1619,#1663,#816,.T.);
#2016=EDGE_CURVE('',#1664,#1650,#817,.T.);
#2017=EDGE_CURVE('',#1665,#1664,#818,.T.);
#2018=EDGE_CURVE('',#1666,#1665,#819,.T.);
#2019=EDGE_CURVE('',#1661,#1666,#820,.T.);
#2020=EDGE_CURVE('',#1663,#1667,#821,.T.);
#2021=EDGE_CURVE('',#1620,#1667,#822,.T.);
#2022=EDGE_CURVE('',#1662,#1668,#823,.T.);
#2023=EDGE_CURVE('',#1667,#1668,#824,.T.);
#2024=EDGE_CURVE('',#1660,#1669,#825,.T.);
#2025=EDGE_CURVE('',#1668,#1669,#826,.T.);
#2026=EDGE_CURVE('',#1669,#1670,#827,.T.);
#2027=EDGE_CURVE('',#1661,#1670,#828,.T.);
#2028=EDGE_CURVE('',#1671,#1649,#829,.T.);
#2029=EDGE_CURVE('',#1664,#1671,#830,.T.);
#2030=EDGE_CURVE('',#1672,#1671,#831,.T.);
#2031=EDGE_CURVE('',#1665,#1672,#832,.T.);
#2032=EDGE_CURVE('',#1673,#1672,#833,.T.);
#2033=EDGE_CURVE('',#1666,#1673,#834,.T.);
#2034=EDGE_CURVE('',#1670,#1673,#835,.T.);
#2035=EDGE_CURVE('',#1674,#1674,#1500,.T.);
#2036=EDGE_CURVE('',#1674,#1675,#1501,.T.);
#2037=EDGE_CURVE('',#1675,#1676,#1502,.T.);
#2038=EDGE_CURVE('',#1676,#1675,#1503,.T.);
#2039=EDGE_CURVE('',#1676,#1677,#836,.T.);
#2040=EDGE_CURVE('',#1678,#1677,#1504,.T.);
#2041=EDGE_CURVE('',#1677,#1678,#1505,.T.);
#2042=EDGE_CURVE('',#1679,#1679,#1506,.T.);
#2043=EDGE_CURVE('',#1678,#1680,#1507,.T.);
#2044=EDGE_CURVE('',#1680,#1680,#1508,.T.);
#2045=EDGE_CURVE('',#1681,#1681,#1509,.T.);
#2046=EDGE_CURVE('',#1679,#1681,#837,.T.);
#2047=EDGE_CURVE('',#1682,#1682,#1510,.T.);
#2048=EDGE_CURVE('',#1682,#1683,#838,.T.);
#2049=EDGE_CURVE('',#1683,#1683,#1511,.T.);
#2050=EDGE_CURVE('',#1684,#1685,#839,.T.);
#2051=EDGE_CURVE('',#1684,#1686,#840,.T.);
#2052=EDGE_CURVE('',#1687,#1686,#841,.T.);
#2053=EDGE_CURVE('',#1685,#1687,#842,.T.);
#2054=EDGE_CURVE('',#1688,#1689,#843,.T.);
#2055=EDGE_CURVE('',#1688,#1690,#844,.T.);
#2056=EDGE_CURVE('',#1691,#1690,#845,.T.);
#2057=EDGE_CURVE('',#1689,#1691,#846,.T.);
#2058=EDGE_CURVE('',#1690,#1687,#847,.T.);
#2059=EDGE_CURVE('',#1686,#1691,#848,.T.);
#2060=EDGE_CURVE('',#1685,#1692,#849,.T.);
#2061=EDGE_CURVE('',#1693,#1692,#850,.T.);
#2062=EDGE_CURVE('',#1684,#1693,#851,.T.);
#2063=EDGE_CURVE('',#1694,#1689,#852,.T.);
#2064=EDGE_CURVE('',#1694,#1695,#853,.T.);
#2065=EDGE_CURVE('',#1695,#1688,#854,.T.);
#2066=EDGE_CURVE('',#1696,#1697,#1512,.T.);
#2067=EDGE_CURVE('',#1697,#1696,#855,.T.);
#2068=EDGE_CURVE('',#1698,#1699,#1513,.T.);
#2069=EDGE_CURVE('',#1699,#1700,#1514,.T.);
#2070=EDGE_CURVE('',#1698,#1700,#856,.T.);
#2071=EDGE_CURVE('',#1701,#1702,#1515,.T.);
#2072=EDGE_CURVE('',#1702,#1703,#1516,.T.);
#2073=EDGE_CURVE('',#1701,#1703,#857,.T.);
#2074=EDGE_CURVE('',#1704,#1705,#1517,.T.);
#2075=EDGE_CURVE('',#1705,#1704,#858,.T.);
#2076=EDGE_CURVE('',#1706,#1694,#859,.T.);
#2077=EDGE_CURVE('',#1707,#1693,#860,.T.);
#2078=EDGE_CURVE('',#1704,#1707,#861,.T.);
#2079=EDGE_CURVE('',#1696,#1705,#862,.T.);
#2080=EDGE_CURVE('',#1706,#1697,#863,.T.);
#2081=EDGE_CURVE('',#1695,#1708,#864,.T.);
#2082=EDGE_CURVE('',#1698,#1708,#865,.T.);
#2083=EDGE_CURVE('',#1701,#1700,#866,.T.);
#2084=EDGE_CURVE('',#1709,#1703,#867,.T.);
#2085=EDGE_CURVE('',#1692,#1709,#868,.T.);
#2086=EDGE_CURVE('',#1703,#1701,#1518,.T.);
#2087=EDGE_CURVE('',#1700,#1698,#1519,.T.);
#2088=EDGE_CURVE('',#1708,#1710,#869,.T.);
#2089=EDGE_CURVE('',#1711,#1710,#870,.T.);
#2090=EDGE_CURVE('',#1711,#1709,#871,.T.);
#2091=EDGE_CURVE('',#1707,#1712,#872,.T.);
#2092=EDGE_CURVE('',#1712,#1713,#873,.T.);
#2093=EDGE_CURVE('',#1713,#1706,#874,.T.);
#2094=EDGE_CURVE('',#1697,#1714,#1520,.T.);
#2095=EDGE_CURVE('',#1714,#1696,#1521,.T.);
#2096=EDGE_CURVE('',#1705,#1715,#1522,.T.);
#2097=EDGE_CURVE('',#1715,#1704,#1523,.T.);
#2098=EDGE_CURVE('',#1716,#1716,#1524,.T.);
#2099=EDGE_CURVE('',#1716,#1702,#875,.T.);
#2100=EDGE_CURVE('',#1717,#1717,#1525,.T.);
#2101=EDGE_CURVE('',#1717,#1715,#876,.T.);
#2102=EDGE_CURVE('',#1718,#1718,#1526,.T.);
#2103=EDGE_CURVE('',#1718,#1699,#877,.T.);
#2104=EDGE_CURVE('',#1719,#1719,#1527,.T.);
#2105=EDGE_CURVE('',#1719,#1714,#878,.T.);
#2106=EDGE_CURVE('',#1711,#1720,#879,.T.);
#2107=EDGE_CURVE('',#1710,#1721,#880,.T.);
#2108=EDGE_CURVE('',#1720,#1721,#881,.T.);
#2109=EDGE_CURVE('',#1720,#1722,#882,.T.);
#2110=EDGE_CURVE('',#1721,#1723,#883,.T.);
#2111=EDGE_CURVE('',#1722,#1723,#884,.T.);
#2112=EDGE_CURVE('',#1722,#1724,#885,.T.);
#2113=EDGE_CURVE('',#1723,#1725,#886,.T.);
#2114=EDGE_CURVE('',#1724,#1725,#887,.T.);
#2115=EDGE_CURVE('',#1726,#1727,#888,.T.);
#2116=EDGE_CURVE('',#1726,#1728,#889,.T.);
#2117=EDGE_CURVE('',#1728,#1729,#890,.T.);
#2118=EDGE_CURVE('',#1727,#1729,#891,.T.);
#2119=EDGE_CURVE('',#1724,#1726,#892,.T.);
#2120=EDGE_CURVE('',#1725,#1728,#893,.T.);
#2121=EDGE_CURVE('',#1730,#1731,#894,.T.);
#2122=EDGE_CURVE('',#1732,#1730,#895,.T.);
#2123=EDGE_CURVE('',#1712,#1732,#896,.T.);
#2124=EDGE_CURVE('',#1727,#1733,#897,.T.);
#2125=EDGE_CURVE('',#1734,#1733,#898,.T.);
#2126=EDGE_CURVE('',#1731,#1734,#899,.T.);
#2127=EDGE_CURVE('',#1732,#1735,#900,.T.);
#2128=EDGE_CURVE('',#1713,#1735,#901,.T.);
#2129=EDGE_CURVE('',#1730,#1736,#902,.T.);
#2130=EDGE_CURVE('',#1735,#1736,#903,.T.);
#2131=EDGE_CURVE('',#1731,#1737,#904,.T.);
#2132=EDGE_CURVE('',#1736,#1737,#905,.T.);
#2133=EDGE_CURVE('',#1738,#1729,#906,.T.);
#2134=EDGE_CURVE('',#1733,#1738,#907,.T.);
#2135=EDGE_CURVE('',#1739,#1738,#908,.T.);
#2136=EDGE_CURVE('',#1734,#1739,#909,.T.);
#2137=EDGE_CURVE('',#1737,#1739,#910,.T.);
#2138=EDGE_CURVE('',#1740,#1741,#1528,.T.);
#2139=EDGE_CURVE('',#1741,#1742,#911,.T.);
#2140=EDGE_CURVE('',#1742,#1743,#1529,.T.);
#2141=EDGE_CURVE('',#1743,#1740,#912,.T.);
#2142=EDGE_CURVE('',#1744,#1742,#913,.T.);
#2143=EDGE_CURVE('',#1745,#1744,#1530,.T.);
#2144=EDGE_CURVE('',#1746,#1745,#914,.T.);
#2145=EDGE_CURVE('',#1747,#1746,#1531,.T.);
#2146=EDGE_CURVE('',#1748,#1747,#915,.T.);
#2147=EDGE_CURVE('',#1749,#1748,#1532,.T.);
#2148=EDGE_CURVE('',#1743,#1749,#916,.T.);
#2149=EDGE_CURVE('',#1750,#1741,#917,.T.);
#2150=EDGE_CURVE('',#1744,#1750,#918,.T.);
#2151=EDGE_CURVE('',#1750,#1751,#1533,.T.);
#2152=EDGE_CURVE('',#1751,#1745,#919,.T.);
#2153=EDGE_CURVE('',#1752,#1753,#1534,.T.);
#2154=EDGE_CURVE('',#1753,#1749,#920,.T.);
#2155=EDGE_CURVE('',#1748,#1752,#921,.T.);
#2156=EDGE_CURVE('',#1754,#1747,#922,.T.);
#2157=EDGE_CURVE('',#1752,#1754,#923,.T.);
#2158=EDGE_CURVE('',#1755,#1754,#1535,.T.);
#2159=EDGE_CURVE('',#1746,#1755,#924,.T.);
#2160=EDGE_CURVE('',#1755,#1751,#925,.T.);
#2161=EDGE_CURVE('',#1740,#1753,#926,.T.);
#2162=EDGE_CURVE('',#1756,#1756,#1536,.T.);
#2163=EDGE_CURVE('',#1756,#1757,#927,.T.);
#2164=EDGE_CURVE('',#1757,#1757,#1537,.T.);
#2165=EDGE_CURVE('',#1758,#1758,#1538,.T.);
#2166=EDGE_CURVE('',#1758,#1759,#928,.T.);
#2167=EDGE_CURVE('',#1759,#1759,#1539,.F.);
#2168=EDGE_CURVE('',#1760,#1760,#1540,.T.);
#2169=EDGE_CURVE('',#1760,#1761,#929,.T.);
#2170=EDGE_CURVE('',#1761,#1761,#1541,.T.);
#2171=EDGE_CURVE('',#1762,#1763,#930,.T.);
#2172=EDGE_CURVE('',#1762,#1764,#931,.T.);
#2173=EDGE_CURVE('',#1765,#1764,#932,.T.);
#2174=EDGE_CURVE('',#1763,#1765,#933,.T.);
#2175=EDGE_CURVE('',#1766,#1762,#934,.T.);
#2176=EDGE_CURVE('',#1766,#1767,#935,.T.);
#2177=EDGE_CURVE('',#1764,#1767,#936,.T.);
#2178=EDGE_CURVE('',#1768,#1766,#937,.T.);
#2179=EDGE_CURVE('',#1768,#1769,#938,.T.);
#2180=EDGE_CURVE('',#1767,#1769,#939,.T.);
#2181=EDGE_CURVE('',#1763,#1768,#940,.T.);
#2182=EDGE_CURVE('',#1769,#1765,#941,.T.);
#2183=EDGE_CURVE('',#1770,#1771,#942,.T.);
#2184=EDGE_CURVE('',#1771,#1772,#943,.T.);
#2185=EDGE_CURVE('',#1772,#1773,#944,.T.);
#2186=EDGE_CURVE('',#1773,#1770,#945,.T.);
#2187=EDGE_CURVE('',#1773,#1774,#946,.T.);
#2188=EDGE_CURVE('',#1775,#1774,#947,.T.);
#2189=EDGE_CURVE('',#1770,#1775,#948,.T.);
#2190=EDGE_CURVE('',#1772,#1776,#949,.T.);
#2191=EDGE_CURVE('',#1777,#1776,#950,.T.);
#2192=EDGE_CURVE('',#1777,#1778,#951,.T.);
#2193=EDGE_CURVE('',#1779,#1778,#952,.T.);
#2194=EDGE_CURVE('',#1779,#1780,#953,.T.);
#2195=EDGE_CURVE('',#1774,#1780,#954,.T.);
#2196=EDGE_CURVE('',#1781,#1782,#955,.T.);
#2197=EDGE_CURVE('',#1782,#1777,#956,.T.);
#2198=EDGE_CURVE('',#1776,#1781,#957,.T.);
#2199=EDGE_CURVE('',#1783,#1782,#958,.T.);
#2200=EDGE_CURVE('',#1778,#1783,#959,.T.);
#2201=EDGE_CURVE('',#1783,#1784,#960,.T.);
#2202=EDGE_CURVE('',#1784,#1779,#961,.T.);
#2203=EDGE_CURVE('',#1785,#1775,#962,.T.);
#2204=EDGE_CURVE('',#1780,#1785,#963,.T.);
#2205=EDGE_CURVE('',#1785,#1784,#964,.T.);
#2206=EDGE_CURVE('',#1781,#1771,#965,.T.);
#2207=EDGE_CURVE('',#1786,#1786,#1542,.T.);
#2208=EDGE_CURVE('',#1786,#1787,#1543,.T.);
#2209=EDGE_CURVE('',#1787,#1787,#1544,.T.);
#2210=EDGE_CURVE('',#1788,#1788,#1545,.T.);
#2211=EDGE_CURVE('',#1788,#1787,#966,.T.);
#2212=EDGE_CURVE('',#1789,#1789,#1546,.T.);
#2213=EDGE_CURVE('',#1790,#1790,#1547,.T.);
#2214=EDGE_CURVE('',#1790,#1791,#1548,.T.);
#2215=EDGE_CURVE('',#1791,#1791,#1549,.T.);
#2216=EDGE_CURVE('',#1792,#1792,#1550,.T.);
#2217=EDGE_CURVE('',#1792,#1791,#967,.T.);
#2218=EDGE_CURVE('',#1793,#1793,#1551,.T.);
#2219=EDGE_CURVE('',#1794,#1794,#1552,.T.);
#2220=EDGE_CURVE('',#1794,#1792,#1553,.T.);
#2221=EDGE_CURVE('',#1793,#1788,#1554,.T.);
#2222=EDGE_CURVE('',#1789,#1795,#1555,.T.);
#2223=EDGE_CURVE('',#1795,#1795,#1556,.T.);
#2224=EDGE_CURVE('',#1795,#1796,#968,.T.);
#2225=EDGE_CURVE('',#1796,#1796,#1557,.T.);
#2226=EDGE_CURVE('',#1797,#1797,#1558,.T.);
#2227=EDGE_CURVE('',#1797,#1798,#969,.T.);
#2228=EDGE_CURVE('',#1798,#1798,#1559,.T.);
#2229=EDGE_CURVE('',#1799,#1799,#1560,.T.);
#2230=EDGE_CURVE('',#1799,#1800,#970,.T.);
#2231=EDGE_CURVE('',#1800,#1800,#1561,.T.);
#2232=EDGE_CURVE('',#1801,#1801,#1562,.T.);
#2233=EDGE_CURVE('',#1801,#1802,#971,.T.);
#2234=EDGE_CURVE('',#1802,#1802,#1563,.T.);
#2235=EDGE_CURVE('',#1803,#1803,#1564,.T.);
#2236=EDGE_CURVE('',#1803,#1804,#972,.T.);
#2237=EDGE_CURVE('',#1804,#1804,#1565,.T.);
#2238=EDGE_CURVE('',#1805,#1806,#973,.T.);
#2239=EDGE_CURVE('',#1806,#1807,#974,.T.);
#2240=EDGE_CURVE('',#1808,#1807,#975,.T.);
#2241=EDGE_CURVE('',#1805,#1808,#976,.T.);
#2242=EDGE_CURVE('',#1809,#1805,#977,.T.);
#2243=EDGE_CURVE('',#1810,#1808,#978,.T.);
#2244=EDGE_CURVE('',#1809,#1810,#979,.T.);
#2245=EDGE_CURVE('',#1811,#1809,#980,.T.);
#2246=EDGE_CURVE('',#1812,#1810,#981,.T.);
#2247=EDGE_CURVE('',#1811,#1812,#982,.T.);
#2248=EDGE_CURVE('',#1813,#1811,#983,.T.);
#2249=EDGE_CURVE('',#1814,#1812,#984,.T.);
#2250=EDGE_CURVE('',#1813,#1814,#985,.T.);
#2251=EDGE_CURVE('',#1815,#1813,#986,.T.);
#2252=EDGE_CURVE('',#1816,#1814,#987,.T.);
#2253=EDGE_CURVE('',#1815,#1816,#988,.T.);
#2254=EDGE_CURVE('',#1817,#1815,#989,.T.);
#2255=EDGE_CURVE('',#1818,#1816,#990,.T.);
#2256=EDGE_CURVE('',#1817,#1818,#991,.T.);
#2257=EDGE_CURVE('',#1819,#1817,#992,.T.);
#2258=EDGE_CURVE('',#1820,#1818,#993,.T.);
#2259=EDGE_CURVE('',#1819,#1820,#994,.T.);
#2260=EDGE_CURVE('',#1821,#1819,#995,.T.);
#2261=EDGE_CURVE('',#1822,#1820,#996,.T.);
#2262=EDGE_CURVE('',#1821,#1822,#997,.T.);
#2263=EDGE_CURVE('',#1823,#1821,#998,.T.);
#2264=EDGE_CURVE('',#1824,#1822,#999,.T.);
#2265=EDGE_CURVE('',#1823,#1824,#1000,.T.);
#2266=EDGE_CURVE('',#1806,#1823,#1001,.T.);
#2267=EDGE_CURVE('',#1807,#1824,#1002,.T.);
#2268=EDGE_CURVE('',#1825,#1825,#1566,.T.);
#2269=EDGE_CURVE('',#1825,#1826,#1003,.T.);
#2270=EDGE_CURVE('',#1826,#1826,#1567,.T.);
#2271=EDGE_CURVE('',#1827,#1827,#1568,.T.);
#2272=EDGE_CURVE('',#1827,#1828,#1004,.T.);
#2273=EDGE_CURVE('',#1828,#1828,#1569,.T.);
#2274=EDGE_CURVE('',#1829,#1829,#1570,.T.);
#2275=EDGE_CURVE('',#1829,#1830,#1005,.T.);
#2276=EDGE_CURVE('',#1830,#1830,#1571,.T.);
#2277=EDGE_CURVE('',#1831,#1831,#1572,.T.);
#2278=EDGE_CURVE('',#1831,#1832,#1006,.T.);
#2279=EDGE_CURVE('',#1832,#1832,#1573,.T.);
#2280=EDGE_CURVE('',#1833,#1834,#1007,.T.);
#2281=EDGE_CURVE('',#1833,#1835,#1008,.T.);
#2282=EDGE_CURVE('',#1835,#1836,#1009,.T.);
#2283=EDGE_CURVE('',#1834,#1836,#1010,.T.);
#2284=EDGE_CURVE('',#1837,#1833,#1011,.T.);
#2285=EDGE_CURVE('',#1837,#1838,#1012,.T.);
#2286=EDGE_CURVE('',#1838,#1835,#1013,.T.);
#2287=EDGE_CURVE('',#1839,#1837,#1014,.T.);
#2288=EDGE_CURVE('',#1839,#1840,#1015,.T.);
#2289=EDGE_CURVE('',#1840,#1838,#1016,.T.);
#2290=EDGE_CURVE('',#1841,#1839,#1017,.T.);
#2291=EDGE_CURVE('',#1841,#1842,#1018,.T.);
#2292=EDGE_CURVE('',#1842,#1840,#1019,.T.);
#2293=EDGE_CURVE('',#1843,#1841,#1020,.T.);
#2294=EDGE_CURVE('',#1843,#1844,#1021,.T.);
#2295=EDGE_CURVE('',#1844,#1842,#1022,.T.);
#2296=EDGE_CURVE('',#1845,#1843,#1023,.T.);
#2297=EDGE_CURVE('',#1845,#1846,#1024,.T.);
#2298=EDGE_CURVE('',#1846,#1844,#1025,.T.);
#2299=EDGE_CURVE('',#1847,#1845,#1026,.T.);
#2300=EDGE_CURVE('',#1847,#1848,#1027,.T.);
#2301=EDGE_CURVE('',#1848,#1846,#1028,.T.);
#2302=EDGE_CURVE('',#1849,#1847,#1029,.T.);
#2303=EDGE_CURVE('',#1849,#1850,#1030,.T.);
#2304=EDGE_CURVE('',#1850,#1848,#1031,.T.);
#2305=EDGE_CURVE('',#1851,#1849,#1032,.T.);
#2306=EDGE_CURVE('',#1851,#1852,#1033,.T.);
#2307=EDGE_CURVE('',#1852,#1850,#1034,.T.);
#2308=EDGE_CURVE('',#1834,#1851,#1035,.T.);
#2309=EDGE_CURVE('',#1836,#1852,#1036,.T.);
#2310=EDGE_CURVE('',#1853,#1853,#1574,.T.);
#2311=EDGE_CURVE('',#1853,#1854,#1037,.T.);
#2312=EDGE_CURVE('',#1854,#1854,#1575,.T.);
#2313=EDGE_CURVE('',#1855,#1855,#1576,.T.);
#2314=EDGE_CURVE('',#1855,#1856,#1038,.T.);
#2315=EDGE_CURVE('',#1856,#1856,#1577,.T.);
#2316=EDGE_CURVE('',#1857,#1857,#1578,.T.);
#2317=EDGE_CURVE('',#1857,#1858,#1039,.T.);
#2318=EDGE_CURVE('',#1858,#1858,#1579,.T.);
#2319=EDGE_CURVE('',#1859,#1859,#1580,.T.);
#2320=EDGE_CURVE('',#1859,#1860,#1040,.T.);
#2321=EDGE_CURVE('',#1860,#1860,#1581,.T.);
#2322=EDGE_CURVE('',#1861,#1862,#1041,.T.);
#2323=EDGE_CURVE('',#1861,#1863,#1042,.T.);
#2324=EDGE_CURVE('',#1863,#1864,#1043,.T.);
#2325=EDGE_CURVE('',#1862,#1864,#1044,.T.);
#2326=EDGE_CURVE('',#1865,#1861,#1045,.T.);
#2327=EDGE_CURVE('',#1865,#1866,#1046,.T.);
#2328=EDGE_CURVE('',#1866,#1863,#1047,.T.);
#2329=EDGE_CURVE('',#1867,#1865,#1048,.T.);
#2330=EDGE_CURVE('',#1867,#1868,#1049,.T.);
#2331=EDGE_CURVE('',#1868,#1866,#1050,.T.);
#2332=EDGE_CURVE('',#1869,#1867,#1051,.T.);
#2333=EDGE_CURVE('',#1869,#1870,#1052,.T.);
#2334=EDGE_CURVE('',#1870,#1868,#1053,.T.);
#2335=EDGE_CURVE('',#1871,#1869,#1054,.T.);
#2336=EDGE_CURVE('',#1871,#1872,#1055,.T.);
#2337=EDGE_CURVE('',#1872,#1870,#1056,.T.);
#2338=EDGE_CURVE('',#1873,#1871,#1057,.T.);
#2339=EDGE_CURVE('',#1873,#1874,#1058,.T.);
#2340=EDGE_CURVE('',#1874,#1872,#1059,.T.);
#2341=EDGE_CURVE('',#1875,#1873,#1060,.T.);
#2342=EDGE_CURVE('',#1875,#1876,#1061,.T.);
#2343=EDGE_CURVE('',#1876,#1874,#1062,.T.);
#2344=EDGE_CURVE('',#1877,#1875,#1063,.T.);
#2345=EDGE_CURVE('',#1877,#1878,#1064,.T.);
#2346=EDGE_CURVE('',#1878,#1876,#1065,.T.);
#2347=EDGE_CURVE('',#1879,#1877,#1066,.T.);
#2348=EDGE_CURVE('',#1879,#1880,#1067,.T.);
#2349=EDGE_CURVE('',#1880,#1878,#1068,.T.);
#2350=EDGE_CURVE('',#1862,#1879,#1069,.T.);
#2351=EDGE_CURVE('',#1864,#1880,#1070,.T.);
#2352=EDGE_CURVE('',#1881,#1881,#1582,.T.);
#2353=EDGE_CURVE('',#1881,#1882,#1071,.T.);
#2354=EDGE_CURVE('',#1882,#1882,#1583,.T.);
#2355=EDGE_CURVE('',#1883,#1883,#1584,.T.);
#2356=EDGE_CURVE('',#1883,#1884,#1072,.T.);
#2357=EDGE_CURVE('',#1884,#1884,#1585,.T.);
#2358=EDGE_CURVE('',#1885,#1885,#1586,.T.);
#2359=EDGE_CURVE('',#1885,#1886,#1073,.T.);
#2360=EDGE_CURVE('',#1886,#1886,#1587,.T.);
#2361=EDGE_CURVE('',#1887,#1887,#1588,.T.);
#2362=EDGE_CURVE('',#1887,#1888,#1074,.T.);
#2363=EDGE_CURVE('',#1888,#1888,#1589,.T.);
#2364=EDGE_CURVE('',#1889,#1890,#1075,.T.);
#2365=EDGE_CURVE('',#1890,#1891,#1076,.T.);
#2366=EDGE_CURVE('',#1892,#1891,#1077,.T.);
#2367=EDGE_CURVE('',#1889,#1892,#1078,.T.);
#2368=EDGE_CURVE('',#1893,#1889,#1079,.T.);
#2369=EDGE_CURVE('',#1894,#1892,#1080,.T.);
#2370=EDGE_CURVE('',#1893,#1894,#1081,.T.);
#2371=EDGE_CURVE('',#1895,#1893,#1082,.T.);
#2372=EDGE_CURVE('',#1896,#1894,#1083,.T.);
#2373=EDGE_CURVE('',#1895,#1896,#1084,.T.);
#2374=EDGE_CURVE('',#1897,#1895,#1085,.T.);
#2375=EDGE_CURVE('',#1898,#1896,#1086,.T.);
#2376=EDGE_CURVE('',#1897,#1898,#1087,.T.);
#2377=EDGE_CURVE('',#1899,#1897,#1088,.T.);
#2378=EDGE_CURVE('',#1900,#1898,#1089,.T.);
#2379=EDGE_CURVE('',#1899,#1900,#1090,.T.);
#2380=EDGE_CURVE('',#1901,#1899,#1091,.T.);
#2381=EDGE_CURVE('',#1902,#1900,#1092,.T.);
#2382=EDGE_CURVE('',#1901,#1902,#1093,.T.);
#2383=EDGE_CURVE('',#1903,#1901,#1094,.T.);
#2384=EDGE_CURVE('',#1904,#1902,#1095,.T.);
#2385=EDGE_CURVE('',#1903,#1904,#1096,.T.);
#2386=EDGE_CURVE('',#1905,#1903,#1097,.T.);
#2387=EDGE_CURVE('',#1906,#1904,#1098,.T.);
#2388=EDGE_CURVE('',#1905,#1906,#1099,.T.);
#2389=EDGE_CURVE('',#1907,#1905,#1100,.T.);
#2390=EDGE_CURVE('',#1908,#1906,#1101,.T.);
#2391=EDGE_CURVE('',#1907,#1908,#1102,.T.);
#2392=EDGE_CURVE('',#1890,#1907,#1103,.T.);
#2393=EDGE_CURVE('',#1891,#1908,#1104,.T.);
#2394=ORIENTED_EDGE('',*,*,#1909,.F.);
#2395=ORIENTED_EDGE('',*,*,#1910,.T.);
#2396=ORIENTED_EDGE('',*,*,#1911,.F.);
#2397=ORIENTED_EDGE('',*,*,#1910,.F.);
#2398=ORIENTED_EDGE('',*,*,#1912,.F.);
#2399=ORIENTED_EDGE('',*,*,#1913,.T.);
#2400=ORIENTED_EDGE('',*,*,#1914,.F.);
#2401=ORIENTED_EDGE('',*,*,#1913,.F.);
#2402=ORIENTED_EDGE('',*,*,#1915,.F.);
#2403=ORIENTED_EDGE('',*,*,#1916,.F.);
#2404=ORIENTED_EDGE('',*,*,#1917,.T.);
#2405=ORIENTED_EDGE('',*,*,#1918,.F.);
#2406=ORIENTED_EDGE('',*,*,#1919,.F.);
#2407=ORIENTED_EDGE('',*,*,#1917,.F.);
#2408=ORIENTED_EDGE('',*,*,#1920,.F.);
#2409=ORIENTED_EDGE('',*,*,#1921,.T.);
#2410=ORIENTED_EDGE('',*,*,#1922,.F.);
#2411=ORIENTED_EDGE('',*,*,#1923,.F.);
#2412=ORIENTED_EDGE('',*,*,#1921,.F.);
#2413=ORIENTED_EDGE('',*,*,#1924,.F.);
#2414=ORIENTED_EDGE('',*,*,#1925,.F.);
#2415=ORIENTED_EDGE('',*,*,#1926,.F.);
#2416=ORIENTED_EDGE('',*,*,#1927,.T.);
#2417=ORIENTED_EDGE('',*,*,#1928,.F.);
#2418=ORIENTED_EDGE('',*,*,#1929,.F.);
#2419=ORIENTED_EDGE('',*,*,#1927,.F.);
#2420=ORIENTED_EDGE('',*,*,#1930,.F.);
#2421=ORIENTED_EDGE('',*,*,#1931,.T.);
#2422=ORIENTED_EDGE('',*,*,#1932,.F.);
#2423=ORIENTED_EDGE('',*,*,#1933,.F.);
#2424=ORIENTED_EDGE('',*,*,#1931,.F.);
#2425=ORIENTED_EDGE('',*,*,#1934,.F.);
#2426=ORIENTED_EDGE('',*,*,#1935,.F.);
#2427=ORIENTED_EDGE('',*,*,#1936,.F.);
#2428=ORIENTED_EDGE('',*,*,#1937,.T.);
#2429=ORIENTED_EDGE('',*,*,#1938,.F.);
#2430=ORIENTED_EDGE('',*,*,#1939,.F.);
#2431=ORIENTED_EDGE('',*,*,#1937,.F.);
#2432=ORIENTED_EDGE('',*,*,#1940,.F.);
#2433=ORIENTED_EDGE('',*,*,#1941,.T.);
#2434=ORIENTED_EDGE('',*,*,#1942,.F.);
#2435=ORIENTED_EDGE('',*,*,#1943,.F.);
#2436=ORIENTED_EDGE('',*,*,#1941,.F.);
#2437=ORIENTED_EDGE('',*,*,#1944,.F.);
#2438=ORIENTED_EDGE('',*,*,#1918,.T.);
#2439=ORIENTED_EDGE('',*,*,#1919,.T.);
#2440=ORIENTED_EDGE('',*,*,#1923,.T.);
#2441=ORIENTED_EDGE('',*,*,#1945,.F.);
#2442=ORIENTED_EDGE('',*,*,#1938,.T.);
#2443=ORIENTED_EDGE('',*,*,#1939,.T.);
#2444=ORIENTED_EDGE('',*,*,#1943,.T.);
#2445=ORIENTED_EDGE('',*,*,#1946,.F.);
#2446=ORIENTED_EDGE('',*,*,#1928,.T.);
#2447=ORIENTED_EDGE('',*,*,#1929,.T.);
#2448=ORIENTED_EDGE('',*,*,#1933,.T.);
#2449=ORIENTED_EDGE('',*,*,#1947,.F.);
#2450=ORIENTED_EDGE('',*,*,#1948,.T.);
#2451=ORIENTED_EDGE('',*,*,#1949,.T.);
#2452=ORIENTED_EDGE('',*,*,#1950,.F.);
#2453=ORIENTED_EDGE('',*,*,#1951,.F.);
#2454=ORIENTED_EDGE('',*,*,#1932,.T.);
#2455=ORIENTED_EDGE('',*,*,#1952,.F.);
#2456=ORIENTED_EDGE('',*,*,#1953,.T.);
#2457=ORIENTED_EDGE('',*,*,#1947,.T.);
#2458=ORIENTED_EDGE('',*,*,#1925,.T.);
#2459=ORIENTED_EDGE('',*,*,#1946,.T.);
#2460=ORIENTED_EDGE('',*,*,#1942,.T.);
#2461=ORIENTED_EDGE('',*,*,#1954,.F.);
#2462=ORIENTED_EDGE('',*,*,#1922,.T.);
#2463=ORIENTED_EDGE('',*,*,#1955,.F.);
#2464=ORIENTED_EDGE('',*,*,#1935,.T.);
#2465=ORIENTED_EDGE('',*,*,#1945,.T.);
#2466=ORIENTED_EDGE('',*,*,#1915,.T.);
#2467=ORIENTED_EDGE('',*,*,#1951,.T.);
#2468=ORIENTED_EDGE('',*,*,#1956,.F.);
#2469=ORIENTED_EDGE('',*,*,#1957,.F.);
#2470=ORIENTED_EDGE('',*,*,#1958,.F.);
#2471=ORIENTED_EDGE('',*,*,#1959,.F.);
#2472=ORIENTED_EDGE('',*,*,#1960,.F.);
#2473=ORIENTED_EDGE('',*,*,#1961,.F.);
#2474=ORIENTED_EDGE('',*,*,#1962,.F.);
#2475=ORIENTED_EDGE('',*,*,#1963,.F.);
#2476=ORIENTED_EDGE('',*,*,#1964,.F.);
#2477=ORIENTED_EDGE('',*,*,#1965,.T.);
#2478=ORIENTED_EDGE('',*,*,#1966,.F.);
#2479=ORIENTED_EDGE('',*,*,#1965,.F.);
#2480=ORIENTED_EDGE('',*,*,#1967,.F.);
#2481=ORIENTED_EDGE('',*,*,#1959,.T.);
#2482=ORIENTED_EDGE('',*,*,#1968,.F.);
#2483=ORIENTED_EDGE('',*,*,#1969,.F.);
#2484=ORIENTED_EDGE('',*,*,#1970,.F.);
#2485=ORIENTED_EDGE('',*,*,#1971,.F.);
#2486=ORIENTED_EDGE('',*,*,#1972,.F.);
#2487=ORIENTED_EDGE('',*,*,#1973,.F.);
#2488=ORIENTED_EDGE('',*,*,#1974,.F.);
#2489=ORIENTED_EDGE('',*,*,#1975,.T.);
#2490=ORIENTED_EDGE('',*,*,#1976,.F.);
#2491=ORIENTED_EDGE('',*,*,#1975,.F.);
#2492=ORIENTED_EDGE('',*,*,#1977,.F.);
#2493=ORIENTED_EDGE('',*,*,#1969,.T.);
#2494=ORIENTED_EDGE('',*,*,#1978,.F.);
#2495=ORIENTED_EDGE('',*,*,#1979,.F.);
#2496=ORIENTED_EDGE('',*,*,#1980,.F.);
#2497=ORIENTED_EDGE('',*,*,#1981,.F.);
#2498=ORIENTED_EDGE('',*,*,#1982,.F.);
#2499=ORIENTED_EDGE('',*,*,#1983,.F.);
#2500=ORIENTED_EDGE('',*,*,#1984,.F.);
#2501=ORIENTED_EDGE('',*,*,#1985,.T.);
#2502=ORIENTED_EDGE('',*,*,#1986,.F.);
#2503=ORIENTED_EDGE('',*,*,#1985,.F.);
#2504=ORIENTED_EDGE('',*,*,#1987,.F.);
#2505=ORIENTED_EDGE('',*,*,#1979,.T.);
#2506=ORIENTED_EDGE('',*,*,#1981,.T.);
#2507=ORIENTED_EDGE('',*,*,#1988,.T.);
#2508=ORIENTED_EDGE('',*,*,#1989,.F.);
#2509=ORIENTED_EDGE('',*,*,#1990,.F.);
#2510=ORIENTED_EDGE('',*,*,#1971,.T.);
#2511=ORIENTED_EDGE('',*,*,#1991,.T.);
#2512=ORIENTED_EDGE('',*,*,#1983,.T.);
#2513=ORIENTED_EDGE('',*,*,#1992,.F.);
#2514=ORIENTED_EDGE('',*,*,#1963,.T.);
#2515=ORIENTED_EDGE('',*,*,#1993,.F.);
#2516=ORIENTED_EDGE('',*,*,#1994,.T.);
#2517=ORIENTED_EDGE('',*,*,#1995,.T.);
#2518=ORIENTED_EDGE('',*,*,#1961,.T.);
#2519=ORIENTED_EDGE('',*,*,#1996,.T.);
#2520=ORIENTED_EDGE('',*,*,#1973,.T.);
#2521=ORIENTED_EDGE('',*,*,#1997,.F.);
#2522=ORIENTED_EDGE('',*,*,#1916,.T.);
#2523=ORIENTED_EDGE('',*,*,#1957,.T.);
#2524=ORIENTED_EDGE('',*,*,#1998,.F.);
#2525=ORIENTED_EDGE('',*,*,#1988,.F.);
#2526=ORIENTED_EDGE('',*,*,#1980,.T.);
#2527=ORIENTED_EDGE('',*,*,#1987,.T.);
#2528=ORIENTED_EDGE('',*,*,#1984,.T.);
#2529=ORIENTED_EDGE('',*,*,#1991,.F.);
#2530=ORIENTED_EDGE('',*,*,#1970,.T.);
#2531=ORIENTED_EDGE('',*,*,#1977,.T.);
#2532=ORIENTED_EDGE('',*,*,#1974,.T.);
#2533=ORIENTED_EDGE('',*,*,#1996,.F.);
#2534=ORIENTED_EDGE('',*,*,#1960,.T.);
#2535=ORIENTED_EDGE('',*,*,#1967,.T.);
#2536=ORIENTED_EDGE('',*,*,#1964,.T.);
#2537=ORIENTED_EDGE('',*,*,#1995,.F.);
#2538=ORIENTED_EDGE('',*,*,#1999,.T.);
#2539=ORIENTED_EDGE('',*,*,#1952,.T.);
#2540=ORIENTED_EDGE('',*,*,#1934,.T.);
#2541=ORIENTED_EDGE('',*,*,#1930,.T.);
#2542=ORIENTED_EDGE('',*,*,#1926,.T.);
#2543=ORIENTED_EDGE('',*,*,#1954,.T.);
#2544=ORIENTED_EDGE('',*,*,#1944,.T.);
#2545=ORIENTED_EDGE('',*,*,#1940,.T.);
#2546=ORIENTED_EDGE('',*,*,#1936,.T.);
#2547=ORIENTED_EDGE('',*,*,#1955,.T.);
#2548=ORIENTED_EDGE('',*,*,#1924,.T.);
#2549=ORIENTED_EDGE('',*,*,#1920,.T.);
#2550=ORIENTED_EDGE('',*,*,#2000,.F.);
#2551=ORIENTED_EDGE('',*,*,#2001,.F.);
#2552=ORIENTED_EDGE('',*,*,#2002,.F.);
#2553=ORIENTED_EDGE('',*,*,#2003,.F.);
#2554=ORIENTED_EDGE('',*,*,#1914,.T.);
#2555=ORIENTED_EDGE('',*,*,#2003,.T.);
#2556=ORIENTED_EDGE('',*,*,#2004,.F.);
#2557=ORIENTED_EDGE('',*,*,#2005,.T.);
#2558=ORIENTED_EDGE('',*,*,#2006,.T.);
#2559=ORIENTED_EDGE('',*,*,#2002,.T.);
#2560=ORIENTED_EDGE('',*,*,#2007,.F.);
#2561=ORIENTED_EDGE('',*,*,#2008,.T.);
#2562=ORIENTED_EDGE('',*,*,#2004,.T.);
#2563=ORIENTED_EDGE('',*,*,#2001,.T.);
#2564=ORIENTED_EDGE('',*,*,#2009,.F.);
#2565=ORIENTED_EDGE('',*,*,#2010,.T.);
#2566=ORIENTED_EDGE('',*,*,#2007,.T.);
#2567=ORIENTED_EDGE('',*,*,#2011,.T.);
#2568=ORIENTED_EDGE('',*,*,#2005,.F.);
#2569=ORIENTED_EDGE('',*,*,#2008,.F.);
#2570=ORIENTED_EDGE('',*,*,#2010,.F.);
#2571=ORIENTED_EDGE('',*,*,#1909,.T.);
#2572=ORIENTED_EDGE('',*,*,#2012,.F.);
#2573=ORIENTED_EDGE('',*,*,#2013,.F.);
#2574=ORIENTED_EDGE('',*,*,#2014,.F.);
#2575=ORIENTED_EDGE('',*,*,#2015,.F.);
#2576=ORIENTED_EDGE('',*,*,#1948,.F.);
#2577=ORIENTED_EDGE('',*,*,#1953,.F.);
#2578=ORIENTED_EDGE('',*,*,#1999,.F.);
#2579=ORIENTED_EDGE('',*,*,#1994,.F.);
#2580=ORIENTED_EDGE('',*,*,#2016,.F.);
#2581=ORIENTED_EDGE('',*,*,#2017,.F.);
#2582=ORIENTED_EDGE('',*,*,#2018,.F.);
#2583=ORIENTED_EDGE('',*,*,#2019,.F.);
#2584=ORIENTED_EDGE('',*,*,#1911,.T.);
#2585=ORIENTED_EDGE('',*,*,#2015,.T.);
#2586=ORIENTED_EDGE('',*,*,#2020,.T.);
#2587=ORIENTED_EDGE('',*,*,#2021,.F.);
#2588=ORIENTED_EDGE('',*,*,#1949,.F.);
#2589=ORIENTED_EDGE('',*,*,#2014,.T.);
#2590=ORIENTED_EDGE('',*,*,#2022,.T.);
#2591=ORIENTED_EDGE('',*,*,#2023,.F.);
#2592=ORIENTED_EDGE('',*,*,#2020,.F.);
#2593=ORIENTED_EDGE('',*,*,#2013,.T.);
#2594=ORIENTED_EDGE('',*,*,#2024,.T.);
#2595=ORIENTED_EDGE('',*,*,#2025,.F.);
#2596=ORIENTED_EDGE('',*,*,#2022,.F.);
#2597=ORIENTED_EDGE('',*,*,#2026,.F.);
#2598=ORIENTED_EDGE('',*,*,#2024,.F.);
#2599=ORIENTED_EDGE('',*,*,#2012,.T.);
#2600=ORIENTED_EDGE('',*,*,#2027,.T.);
#2601=ORIENTED_EDGE('',*,*,#2006,.F.);
#2602=ORIENTED_EDGE('',*,*,#2011,.F.);
#2603=ORIENTED_EDGE('',*,*,#2009,.T.);
#2604=ORIENTED_EDGE('',*,*,#2000,.T.);
#2605=ORIENTED_EDGE('',*,*,#1958,.T.);
#2606=ORIENTED_EDGE('',*,*,#1997,.T.);
#2607=ORIENTED_EDGE('',*,*,#1972,.T.);
#2608=ORIENTED_EDGE('',*,*,#1976,.T.);
#2609=ORIENTED_EDGE('',*,*,#1968,.T.);
#2610=ORIENTED_EDGE('',*,*,#1992,.T.);
#2611=ORIENTED_EDGE('',*,*,#1982,.T.);
#2612=ORIENTED_EDGE('',*,*,#1986,.T.);
#2613=ORIENTED_EDGE('',*,*,#1978,.T.);
#2614=ORIENTED_EDGE('',*,*,#1990,.T.);
#2615=ORIENTED_EDGE('',*,*,#2028,.F.);
#2616=ORIENTED_EDGE('',*,*,#2029,.F.);
#2617=ORIENTED_EDGE('',*,*,#2016,.T.);
#2618=ORIENTED_EDGE('',*,*,#1993,.T.);
#2619=ORIENTED_EDGE('',*,*,#1962,.T.);
#2620=ORIENTED_EDGE('',*,*,#1966,.T.);
#2621=ORIENTED_EDGE('',*,*,#2017,.T.);
#2622=ORIENTED_EDGE('',*,*,#2029,.T.);
#2623=ORIENTED_EDGE('',*,*,#2030,.F.);
#2624=ORIENTED_EDGE('',*,*,#2031,.F.);
#2625=ORIENTED_EDGE('',*,*,#2018,.T.);
#2626=ORIENTED_EDGE('',*,*,#2031,.T.);
#2627=ORIENTED_EDGE('',*,*,#2032,.F.);
#2628=ORIENTED_EDGE('',*,*,#2033,.F.);
#2629=ORIENTED_EDGE('',*,*,#2019,.T.);
#2630=ORIENTED_EDGE('',*,*,#2033,.T.);
#2631=ORIENTED_EDGE('',*,*,#2034,.F.);
#2632=ORIENTED_EDGE('',*,*,#2027,.F.);
#2633=ORIENTED_EDGE('',*,*,#2026,.T.);
#2634=ORIENTED_EDGE('',*,*,#2034,.T.);
#2635=ORIENTED_EDGE('',*,*,#2032,.T.);
#2636=ORIENTED_EDGE('',*,*,#2030,.T.);
#2637=ORIENTED_EDGE('',*,*,#2028,.T.);
#2638=ORIENTED_EDGE('',*,*,#1989,.T.);
#2639=ORIENTED_EDGE('',*,*,#1998,.T.);
#2640=ORIENTED_EDGE('',*,*,#1956,.T.);
#2641=ORIENTED_EDGE('',*,*,#1950,.T.);
#2642=ORIENTED_EDGE('',*,*,#2021,.T.);
#2643=ORIENTED_EDGE('',*,*,#2023,.T.);
#2644=ORIENTED_EDGE('',*,*,#2025,.T.);
#2645=ORIENTED_EDGE('',*,*,#1912,.T.);
#2646=ORIENTED_EDGE('',*,*,#2035,.T.);
#2647=ORIENTED_EDGE('',*,*,#2036,.T.);
#2648=ORIENTED_EDGE('',*,*,#2037,.T.);
#2649=ORIENTED_EDGE('',*,*,#2038,.T.);
#2650=ORIENTED_EDGE('',*,*,#2036,.F.);
#2651=ORIENTED_EDGE('',*,*,#2038,.F.);
#2652=ORIENTED_EDGE('',*,*,#2039,.T.);
#2653=ORIENTED_EDGE('',*,*,#2040,.F.);
#2654=ORIENTED_EDGE('',*,*,#2041,.F.);
#2655=ORIENTED_EDGE('',*,*,#2039,.F.);
#2656=ORIENTED_EDGE('',*,*,#2037,.F.);
#2657=ORIENTED_EDGE('',*,*,#2035,.F.);
#2658=ORIENTED_EDGE('',*,*,#2042,.T.);
#2659=ORIENTED_EDGE('',*,*,#2041,.T.);
#2660=ORIENTED_EDGE('',*,*,#2043,.T.);
#2661=ORIENTED_EDGE('',*,*,#2044,.T.);
#2662=ORIENTED_EDGE('',*,*,#2043,.F.);
#2663=ORIENTED_EDGE('',*,*,#2040,.T.);
#2664=ORIENTED_EDGE('',*,*,#2044,.F.);
#2665=ORIENTED_EDGE('',*,*,#2045,.F.);
#2666=ORIENTED_EDGE('',*,*,#2042,.F.);
#2667=ORIENTED_EDGE('',*,*,#2046,.T.);
#2668=ORIENTED_EDGE('',*,*,#2045,.T.);
#2669=ORIENTED_EDGE('',*,*,#2046,.F.);
#2670=ORIENTED_EDGE('',*,*,#2047,.F.);
#2671=ORIENTED_EDGE('',*,*,#2048,.T.);
#2672=ORIENTED_EDGE('',*,*,#2049,.F.);
#2673=ORIENTED_EDGE('',*,*,#2048,.F.);
#2674=ORIENTED_EDGE('',*,*,#2050,.F.);
#2675=ORIENTED_EDGE('',*,*,#2051,.T.);
#2676=ORIENTED_EDGE('',*,*,#2052,.F.);
#2677=ORIENTED_EDGE('',*,*,#2053,.F.);
#2678=ORIENTED_EDGE('',*,*,#2049,.T.);
#2679=ORIENTED_EDGE('',*,*,#2054,.F.);
#2680=ORIENTED_EDGE('',*,*,#2055,.T.);
#2681=ORIENTED_EDGE('',*,*,#2056,.F.);
#2682=ORIENTED_EDGE('',*,*,#2057,.F.);
#2683=ORIENTED_EDGE('',*,*,#2047,.T.);
#2684=ORIENTED_EDGE('',*,*,#2056,.T.);
#2685=ORIENTED_EDGE('',*,*,#2058,.T.);
#2686=ORIENTED_EDGE('',*,*,#2052,.T.);
#2687=ORIENTED_EDGE('',*,*,#2059,.T.);
#2688=ORIENTED_EDGE('',*,*,#2050,.T.);
#2689=ORIENTED_EDGE('',*,*,#2060,.T.);
#2690=ORIENTED_EDGE('',*,*,#2061,.F.);
#2691=ORIENTED_EDGE('',*,*,#2062,.F.);
#2692=ORIENTED_EDGE('',*,*,#2054,.T.);
#2693=ORIENTED_EDGE('',*,*,#2063,.F.);
#2694=ORIENTED_EDGE('',*,*,#2064,.T.);
#2695=ORIENTED_EDGE('',*,*,#2065,.T.);
#2696=ORIENTED_EDGE('',*,*,#2066,.T.);
#2697=ORIENTED_EDGE('',*,*,#2067,.T.);
#2698=ORIENTED_EDGE('',*,*,#2068,.T.);
#2699=ORIENTED_EDGE('',*,*,#2069,.T.);
#2700=ORIENTED_EDGE('',*,*,#2070,.F.);
#2701=ORIENTED_EDGE('',*,*,#2071,.T.);
#2702=ORIENTED_EDGE('',*,*,#2072,.T.);
#2703=ORIENTED_EDGE('',*,*,#2073,.F.);
#2704=ORIENTED_EDGE('',*,*,#2074,.T.);
#2705=ORIENTED_EDGE('',*,*,#2075,.T.);
#2706=ORIENTED_EDGE('',*,*,#2076,.T.);
#2707=ORIENTED_EDGE('',*,*,#2063,.T.);
#2708=ORIENTED_EDGE('',*,*,#2057,.T.);
#2709=ORIENTED_EDGE('',*,*,#2059,.F.);
#2710=ORIENTED_EDGE('',*,*,#2051,.F.);
#2711=ORIENTED_EDGE('',*,*,#2062,.T.);
#2712=ORIENTED_EDGE('',*,*,#2077,.F.);
#2713=ORIENTED_EDGE('',*,*,#2078,.F.);
#2714=ORIENTED_EDGE('',*,*,#2075,.F.);
#2715=ORIENTED_EDGE('',*,*,#2079,.F.);
#2716=ORIENTED_EDGE('',*,*,#2067,.F.);
#2717=ORIENTED_EDGE('',*,*,#2080,.F.);
#2718=ORIENTED_EDGE('',*,*,#2081,.T.);
#2719=ORIENTED_EDGE('',*,*,#2082,.F.);
#2720=ORIENTED_EDGE('',*,*,#2070,.T.);
#2721=ORIENTED_EDGE('',*,*,#2083,.F.);
#2722=ORIENTED_EDGE('',*,*,#2073,.T.);
#2723=ORIENTED_EDGE('',*,*,#2084,.F.);
#2724=ORIENTED_EDGE('',*,*,#2085,.F.);
#2725=ORIENTED_EDGE('',*,*,#2060,.F.);
#2726=ORIENTED_EDGE('',*,*,#2053,.T.);
#2727=ORIENTED_EDGE('',*,*,#2058,.F.);
#2728=ORIENTED_EDGE('',*,*,#2055,.F.);
#2729=ORIENTED_EDGE('',*,*,#2065,.F.);
#2730=ORIENTED_EDGE('',*,*,#2084,.T.);
#2731=ORIENTED_EDGE('',*,*,#2086,.T.);
#2732=ORIENTED_EDGE('',*,*,#2083,.T.);
#2733=ORIENTED_EDGE('',*,*,#2087,.T.);
#2734=ORIENTED_EDGE('',*,*,#2082,.T.);
#2735=ORIENTED_EDGE('',*,*,#2088,.T.);
#2736=ORIENTED_EDGE('',*,*,#2089,.F.);
#2737=ORIENTED_EDGE('',*,*,#2090,.T.);
#2738=ORIENTED_EDGE('',*,*,#2078,.T.);
#2739=ORIENTED_EDGE('',*,*,#2091,.T.);
#2740=ORIENTED_EDGE('',*,*,#2092,.T.);
#2741=ORIENTED_EDGE('',*,*,#2093,.T.);
#2742=ORIENTED_EDGE('',*,*,#2080,.T.);
#2743=ORIENTED_EDGE('',*,*,#2094,.T.);
#2744=ORIENTED_EDGE('',*,*,#2095,.T.);
#2745=ORIENTED_EDGE('',*,*,#2079,.T.);
#2746=ORIENTED_EDGE('',*,*,#2096,.T.);
#2747=ORIENTED_EDGE('',*,*,#2097,.T.);
#2748=ORIENTED_EDGE('',*,*,#2098,.F.);
#2749=ORIENTED_EDGE('',*,*,#2099,.T.);
#2750=ORIENTED_EDGE('',*,*,#2071,.F.);
#2751=ORIENTED_EDGE('',*,*,#2086,.F.);
#2752=ORIENTED_EDGE('',*,*,#2072,.F.);
#2753=ORIENTED_EDGE('',*,*,#2099,.F.);
#2754=ORIENTED_EDGE('',*,*,#2100,.F.);
#2755=ORIENTED_EDGE('',*,*,#2101,.T.);
#2756=ORIENTED_EDGE('',*,*,#2096,.F.);
#2757=ORIENTED_EDGE('',*,*,#2074,.F.);
#2758=ORIENTED_EDGE('',*,*,#2097,.F.);
#2759=ORIENTED_EDGE('',*,*,#2101,.F.);
#2760=ORIENTED_EDGE('',*,*,#2102,.F.);
#2761=ORIENTED_EDGE('',*,*,#2103,.T.);
#2762=ORIENTED_EDGE('',*,*,#2068,.F.);
#2763=ORIENTED_EDGE('',*,*,#2087,.F.);
#2764=ORIENTED_EDGE('',*,*,#2069,.F.);
#2765=ORIENTED_EDGE('',*,*,#2103,.F.);
#2766=ORIENTED_EDGE('',*,*,#2104,.F.);
#2767=ORIENTED_EDGE('',*,*,#2105,.T.);
#2768=ORIENTED_EDGE('',*,*,#2094,.F.);
#2769=ORIENTED_EDGE('',*,*,#2066,.F.);
#2770=ORIENTED_EDGE('',*,*,#2095,.F.);
#2771=ORIENTED_EDGE('',*,*,#2105,.F.);
#2772=ORIENTED_EDGE('',*,*,#2106,.F.);
#2773=ORIENTED_EDGE('',*,*,#2089,.T.);
#2774=ORIENTED_EDGE('',*,*,#2107,.T.);
#2775=ORIENTED_EDGE('',*,*,#2108,.F.);
#2776=ORIENTED_EDGE('',*,*,#2109,.F.);
#2777=ORIENTED_EDGE('',*,*,#2108,.T.);
#2778=ORIENTED_EDGE('',*,*,#2110,.T.);
#2779=ORIENTED_EDGE('',*,*,#2111,.F.);
#2780=ORIENTED_EDGE('',*,*,#2112,.F.);
#2781=ORIENTED_EDGE('',*,*,#2111,.T.);
#2782=ORIENTED_EDGE('',*,*,#2113,.T.);
#2783=ORIENTED_EDGE('',*,*,#2114,.F.);
#2784=ORIENTED_EDGE('',*,*,#2115,.F.);
#2785=ORIENTED_EDGE('',*,*,#2116,.T.);
#2786=ORIENTED_EDGE('',*,*,#2117,.T.);
#2787=ORIENTED_EDGE('',*,*,#2118,.F.);
#2788=ORIENTED_EDGE('',*,*,#2119,.F.);
#2789=ORIENTED_EDGE('',*,*,#2114,.T.);
#2790=ORIENTED_EDGE('',*,*,#2120,.T.);
#2791=ORIENTED_EDGE('',*,*,#2116,.F.);
#2792=ORIENTED_EDGE('',*,*,#2121,.F.);
#2793=ORIENTED_EDGE('',*,*,#2122,.F.);
#2794=ORIENTED_EDGE('',*,*,#2123,.F.);
#2795=ORIENTED_EDGE('',*,*,#2091,.F.);
#2796=ORIENTED_EDGE('',*,*,#2077,.T.);
#2797=ORIENTED_EDGE('',*,*,#2061,.T.);
#2798=ORIENTED_EDGE('',*,*,#2085,.T.);
#2799=ORIENTED_EDGE('',*,*,#2090,.F.);
#2800=ORIENTED_EDGE('',*,*,#2106,.T.);
#2801=ORIENTED_EDGE('',*,*,#2109,.T.);
#2802=ORIENTED_EDGE('',*,*,#2112,.T.);
#2803=ORIENTED_EDGE('',*,*,#2119,.T.);
#2804=ORIENTED_EDGE('',*,*,#2115,.T.);
#2805=ORIENTED_EDGE('',*,*,#2124,.T.);
#2806=ORIENTED_EDGE('',*,*,#2125,.F.);
#2807=ORIENTED_EDGE('',*,*,#2126,.F.);
#2808=ORIENTED_EDGE('',*,*,#2123,.T.);
#2809=ORIENTED_EDGE('',*,*,#2127,.T.);
#2810=ORIENTED_EDGE('',*,*,#2128,.F.);
#2811=ORIENTED_EDGE('',*,*,#2092,.F.);
#2812=ORIENTED_EDGE('',*,*,#2122,.T.);
#2813=ORIENTED_EDGE('',*,*,#2129,.T.);
#2814=ORIENTED_EDGE('',*,*,#2130,.F.);
#2815=ORIENTED_EDGE('',*,*,#2127,.F.);
#2816=ORIENTED_EDGE('',*,*,#2121,.T.);
#2817=ORIENTED_EDGE('',*,*,#2131,.T.);
#2818=ORIENTED_EDGE('',*,*,#2132,.F.);
#2819=ORIENTED_EDGE('',*,*,#2129,.F.);
#2820=ORIENTED_EDGE('',*,*,#2124,.F.);
#2821=ORIENTED_EDGE('',*,*,#2118,.T.);
#2822=ORIENTED_EDGE('',*,*,#2133,.F.);
#2823=ORIENTED_EDGE('',*,*,#2134,.F.);
#2824=ORIENTED_EDGE('',*,*,#2098,.T.);
#2825=ORIENTED_EDGE('',*,*,#2100,.T.);
#2826=ORIENTED_EDGE('',*,*,#2102,.T.);
#2827=ORIENTED_EDGE('',*,*,#2104,.T.);
#2828=ORIENTED_EDGE('',*,*,#2125,.T.);
#2829=ORIENTED_EDGE('',*,*,#2134,.T.);
#2830=ORIENTED_EDGE('',*,*,#2135,.F.);
#2831=ORIENTED_EDGE('',*,*,#2136,.F.);
#2832=ORIENTED_EDGE('',*,*,#2126,.T.);
#2833=ORIENTED_EDGE('',*,*,#2136,.T.);
#2834=ORIENTED_EDGE('',*,*,#2137,.F.);
#2835=ORIENTED_EDGE('',*,*,#2131,.F.);
#2836=ORIENTED_EDGE('',*,*,#2132,.T.);
#2837=ORIENTED_EDGE('',*,*,#2137,.T.);
#2838=ORIENTED_EDGE('',*,*,#2135,.T.);
#2839=ORIENTED_EDGE('',*,*,#2133,.T.);
#2840=ORIENTED_EDGE('',*,*,#2117,.F.);
#2841=ORIENTED_EDGE('',*,*,#2120,.F.);
#2842=ORIENTED_EDGE('',*,*,#2113,.F.);
#2843=ORIENTED_EDGE('',*,*,#2110,.F.);
#2844=ORIENTED_EDGE('',*,*,#2107,.F.);
#2845=ORIENTED_EDGE('',*,*,#2088,.F.);
#2846=ORIENTED_EDGE('',*,*,#2081,.F.);
#2847=ORIENTED_EDGE('',*,*,#2064,.F.);
#2848=ORIENTED_EDGE('',*,*,#2076,.F.);
#2849=ORIENTED_EDGE('',*,*,#2093,.F.);
#2850=ORIENTED_EDGE('',*,*,#2128,.T.);
#2851=ORIENTED_EDGE('',*,*,#2130,.T.);
#2852=ORIENTED_EDGE('',*,*,#2138,.T.);
#2853=ORIENTED_EDGE('',*,*,#2139,.T.);
#2854=ORIENTED_EDGE('',*,*,#2140,.T.);
#2855=ORIENTED_EDGE('',*,*,#2141,.T.);
#2856=ORIENTED_EDGE('',*,*,#2140,.F.);
#2857=ORIENTED_EDGE('',*,*,#2142,.F.);
#2858=ORIENTED_EDGE('',*,*,#2143,.F.);
#2859=ORIENTED_EDGE('',*,*,#2144,.F.);
#2860=ORIENTED_EDGE('',*,*,#2145,.F.);
#2861=ORIENTED_EDGE('',*,*,#2146,.F.);
#2862=ORIENTED_EDGE('',*,*,#2147,.F.);
#2863=ORIENTED_EDGE('',*,*,#2148,.F.);
#2864=ORIENTED_EDGE('',*,*,#2139,.F.);
#2865=ORIENTED_EDGE('',*,*,#2149,.F.);
#2866=ORIENTED_EDGE('',*,*,#2150,.F.);
#2867=ORIENTED_EDGE('',*,*,#2142,.T.);
#2868=ORIENTED_EDGE('',*,*,#2151,.T.);
#2869=ORIENTED_EDGE('',*,*,#2152,.T.);
#2870=ORIENTED_EDGE('',*,*,#2143,.T.);
#2871=ORIENTED_EDGE('',*,*,#2150,.T.);
#2872=ORIENTED_EDGE('',*,*,#2153,.T.);
#2873=ORIENTED_EDGE('',*,*,#2154,.T.);
#2874=ORIENTED_EDGE('',*,*,#2147,.T.);
#2875=ORIENTED_EDGE('',*,*,#2155,.T.);
#2876=ORIENTED_EDGE('',*,*,#2155,.F.);
#2877=ORIENTED_EDGE('',*,*,#2146,.T.);
#2878=ORIENTED_EDGE('',*,*,#2156,.F.);
#2879=ORIENTED_EDGE('',*,*,#2157,.F.);
#2880=ORIENTED_EDGE('',*,*,#2158,.T.);
#2881=ORIENTED_EDGE('',*,*,#2156,.T.);
#2882=ORIENTED_EDGE('',*,*,#2145,.T.);
#2883=ORIENTED_EDGE('',*,*,#2159,.T.);
#2884=ORIENTED_EDGE('',*,*,#2152,.F.);
#2885=ORIENTED_EDGE('',*,*,#2160,.F.);
#2886=ORIENTED_EDGE('',*,*,#2159,.F.);
#2887=ORIENTED_EDGE('',*,*,#2144,.T.);
#2888=ORIENTED_EDGE('',*,*,#2141,.F.);
#2889=ORIENTED_EDGE('',*,*,#2148,.T.);
#2890=ORIENTED_EDGE('',*,*,#2154,.F.);
#2891=ORIENTED_EDGE('',*,*,#2161,.F.);
#2892=ORIENTED_EDGE('',*,*,#2138,.F.);
#2893=ORIENTED_EDGE('',*,*,#2161,.T.);
#2894=ORIENTED_EDGE('',*,*,#2153,.F.);
#2895=ORIENTED_EDGE('',*,*,#2157,.T.);
#2896=ORIENTED_EDGE('',*,*,#2158,.F.);
#2897=ORIENTED_EDGE('',*,*,#2160,.T.);
#2898=ORIENTED_EDGE('',*,*,#2151,.F.);
#2899=ORIENTED_EDGE('',*,*,#2149,.T.);
#2900=ORIENTED_EDGE('',*,*,#2162,.F.);
#2901=ORIENTED_EDGE('',*,*,#2163,.T.);
#2902=ORIENTED_EDGE('',*,*,#2164,.F.);
#2903=ORIENTED_EDGE('',*,*,#2163,.F.);
#2904=ORIENTED_EDGE('',*,*,#2162,.T.);
#2905=ORIENTED_EDGE('',*,*,#2165,.F.);
#2906=ORIENTED_EDGE('',*,*,#2166,.T.);
#2907=ORIENTED_EDGE('',*,*,#2167,.F.);
#2908=ORIENTED_EDGE('',*,*,#2166,.F.);
#2909=ORIENTED_EDGE('',*,*,#2167,.T.);
#2910=ORIENTED_EDGE('',*,*,#2164,.T.);
#2911=ORIENTED_EDGE('',*,*,#2165,.T.);
#2912=ORIENTED_EDGE('',*,*,#2168,.F.);
#2913=ORIENTED_EDGE('',*,*,#2169,.T.);
#2914=ORIENTED_EDGE('',*,*,#2170,.F.);
#2915=ORIENTED_EDGE('',*,*,#2169,.F.);
#2916=ORIENTED_EDGE('',*,*,#2171,.F.);
#2917=ORIENTED_EDGE('',*,*,#2172,.T.);
#2918=ORIENTED_EDGE('',*,*,#2173,.F.);
#2919=ORIENTED_EDGE('',*,*,#2174,.F.);
#2920=ORIENTED_EDGE('',*,*,#2175,.F.);
#2921=ORIENTED_EDGE('',*,*,#2176,.T.);
#2922=ORIENTED_EDGE('',*,*,#2177,.F.);
#2923=ORIENTED_EDGE('',*,*,#2172,.F.);
#2924=ORIENTED_EDGE('',*,*,#2178,.F.);
#2925=ORIENTED_EDGE('',*,*,#2179,.T.);
#2926=ORIENTED_EDGE('',*,*,#2180,.F.);
#2927=ORIENTED_EDGE('',*,*,#2176,.F.);
#2928=ORIENTED_EDGE('',*,*,#2168,.T.);
#2929=ORIENTED_EDGE('',*,*,#2181,.F.);
#2930=ORIENTED_EDGE('',*,*,#2174,.T.);
#2931=ORIENTED_EDGE('',*,*,#2182,.F.);
#2932=ORIENTED_EDGE('',*,*,#2179,.F.);
#2933=ORIENTED_EDGE('',*,*,#2183,.T.);
#2934=ORIENTED_EDGE('',*,*,#2184,.T.);
#2935=ORIENTED_EDGE('',*,*,#2185,.T.);
#2936=ORIENTED_EDGE('',*,*,#2186,.T.);
#2937=ORIENTED_EDGE('',*,*,#2186,.F.);
#2938=ORIENTED_EDGE('',*,*,#2187,.T.);
#2939=ORIENTED_EDGE('',*,*,#2188,.F.);
#2940=ORIENTED_EDGE('',*,*,#2189,.F.);
#2941=ORIENTED_EDGE('',*,*,#2173,.T.);
#2942=ORIENTED_EDGE('',*,*,#2177,.T.);
#2943=ORIENTED_EDGE('',*,*,#2180,.T.);
#2944=ORIENTED_EDGE('',*,*,#2182,.T.);
#2945=ORIENTED_EDGE('',*,*,#2185,.F.);
#2946=ORIENTED_EDGE('',*,*,#2190,.T.);
#2947=ORIENTED_EDGE('',*,*,#2191,.F.);
#2948=ORIENTED_EDGE('',*,*,#2192,.T.);
#2949=ORIENTED_EDGE('',*,*,#2193,.F.);
#2950=ORIENTED_EDGE('',*,*,#2194,.T.);
#2951=ORIENTED_EDGE('',*,*,#2195,.F.);
#2952=ORIENTED_EDGE('',*,*,#2187,.F.);
#2953=ORIENTED_EDGE('',*,*,#2170,.T.);
#2954=ORIENTED_EDGE('',*,*,#2196,.T.);
#2955=ORIENTED_EDGE('',*,*,#2197,.T.);
#2956=ORIENTED_EDGE('',*,*,#2191,.T.);
#2957=ORIENTED_EDGE('',*,*,#2198,.T.);
#2958=ORIENTED_EDGE('',*,*,#2197,.F.);
#2959=ORIENTED_EDGE('',*,*,#2199,.F.);
#2960=ORIENTED_EDGE('',*,*,#2200,.F.);
#2961=ORIENTED_EDGE('',*,*,#2192,.F.);
#2962=ORIENTED_EDGE('',*,*,#2171,.T.);
#2963=ORIENTED_EDGE('',*,*,#2181,.T.);
#2964=ORIENTED_EDGE('',*,*,#2178,.T.);
#2965=ORIENTED_EDGE('',*,*,#2175,.T.);
#2966=ORIENTED_EDGE('',*,*,#2201,.T.);
#2967=ORIENTED_EDGE('',*,*,#2202,.T.);
#2968=ORIENTED_EDGE('',*,*,#2193,.T.);
#2969=ORIENTED_EDGE('',*,*,#2200,.T.);
#2970=ORIENTED_EDGE('',*,*,#2203,.T.);
#2971=ORIENTED_EDGE('',*,*,#2188,.T.);
#2972=ORIENTED_EDGE('',*,*,#2195,.T.);
#2973=ORIENTED_EDGE('',*,*,#2204,.T.);
#2974=ORIENTED_EDGE('',*,*,#2202,.F.);
#2975=ORIENTED_EDGE('',*,*,#2205,.F.);
#2976=ORIENTED_EDGE('',*,*,#2204,.F.);
#2977=ORIENTED_EDGE('',*,*,#2194,.F.);
#2978=ORIENTED_EDGE('',*,*,#2184,.F.);
#2979=ORIENTED_EDGE('',*,*,#2206,.F.);
#2980=ORIENTED_EDGE('',*,*,#2198,.F.);
#2981=ORIENTED_EDGE('',*,*,#2190,.F.);
#2982=ORIENTED_EDGE('',*,*,#2183,.F.);
#2983=ORIENTED_EDGE('',*,*,#2189,.T.);
#2984=ORIENTED_EDGE('',*,*,#2203,.F.);
#2985=ORIENTED_EDGE('',*,*,#2205,.T.);
#2986=ORIENTED_EDGE('',*,*,#2201,.F.);
#2987=ORIENTED_EDGE('',*,*,#2199,.T.);
#2988=ORIENTED_EDGE('',*,*,#2196,.F.);
#2989=ORIENTED_EDGE('',*,*,#2206,.T.);
#2990=ORIENTED_EDGE('',*,*,#2207,.T.);
#2991=ORIENTED_EDGE('',*,*,#2208,.T.);
#2992=ORIENTED_EDGE('',*,*,#2209,.T.);
#2993=ORIENTED_EDGE('',*,*,#2208,.F.);
#2994=ORIENTED_EDGE('',*,*,#2210,.F.);
#2995=ORIENTED_EDGE('',*,*,#2211,.T.);
#2996=ORIENTED_EDGE('',*,*,#2209,.F.);
#2997=ORIENTED_EDGE('',*,*,#2211,.F.);
#2998=ORIENTED_EDGE('',*,*,#2212,.F.);
#2999=ORIENTED_EDGE('',*,*,#2207,.F.);
#3000=ORIENTED_EDGE('',*,*,#2213,.T.);
#3001=ORIENTED_EDGE('',*,*,#2214,.T.);
#3002=ORIENTED_EDGE('',*,*,#2215,.T.);
#3003=ORIENTED_EDGE('',*,*,#2214,.F.);
#3004=ORIENTED_EDGE('',*,*,#2216,.F.);
#3005=ORIENTED_EDGE('',*,*,#2217,.T.);
#3006=ORIENTED_EDGE('',*,*,#2215,.F.);
#3007=ORIENTED_EDGE('',*,*,#2217,.F.);
#3008=ORIENTED_EDGE('',*,*,#2218,.F.);
#3009=ORIENTED_EDGE('',*,*,#2213,.F.);
#3010=ORIENTED_EDGE('',*,*,#2219,.T.);
#3011=ORIENTED_EDGE('',*,*,#2220,.T.);
#3012=ORIENTED_EDGE('',*,*,#2216,.T.);
#3013=ORIENTED_EDGE('',*,*,#2220,.F.);
#3014=ORIENTED_EDGE('',*,*,#2219,.F.);
#3015=ORIENTED_EDGE('',*,*,#2218,.T.);
#3016=ORIENTED_EDGE('',*,*,#2221,.T.);
#3017=ORIENTED_EDGE('',*,*,#2210,.T.);
#3018=ORIENTED_EDGE('',*,*,#2221,.F.);
#3019=ORIENTED_EDGE('',*,*,#2212,.T.);
#3020=ORIENTED_EDGE('',*,*,#2222,.T.);
#3021=ORIENTED_EDGE('',*,*,#2223,.T.);
#3022=ORIENTED_EDGE('',*,*,#2222,.F.);
#3023=ORIENTED_EDGE('',*,*,#2223,.F.);
#3024=ORIENTED_EDGE('',*,*,#2224,.T.);
#3025=ORIENTED_EDGE('',*,*,#2225,.T.);
#3026=ORIENTED_EDGE('',*,*,#2224,.F.);
#3027=ORIENTED_EDGE('',*,*,#2225,.F.);
#3028=ORIENTED_EDGE('',*,*,#2226,.F.);
#3029=ORIENTED_EDGE('',*,*,#2227,.T.);
#3030=ORIENTED_EDGE('',*,*,#2228,.T.);
#3031=ORIENTED_EDGE('',*,*,#2227,.F.);
#3032=ORIENTED_EDGE('',*,*,#2229,.F.);
#3033=ORIENTED_EDGE('',*,*,#2230,.T.);
#3034=ORIENTED_EDGE('',*,*,#2231,.T.);
#3035=ORIENTED_EDGE('',*,*,#2230,.F.);
#3036=ORIENTED_EDGE('',*,*,#2232,.F.);
#3037=ORIENTED_EDGE('',*,*,#2233,.T.);
#3038=ORIENTED_EDGE('',*,*,#2234,.T.);
#3039=ORIENTED_EDGE('',*,*,#2233,.F.);
#3040=ORIENTED_EDGE('',*,*,#2235,.F.);
#3041=ORIENTED_EDGE('',*,*,#2236,.T.);
#3042=ORIENTED_EDGE('',*,*,#2237,.T.);
#3043=ORIENTED_EDGE('',*,*,#2236,.F.);
#3044=ORIENTED_EDGE('',*,*,#2238,.T.);
#3045=ORIENTED_EDGE('',*,*,#2239,.T.);
#3046=ORIENTED_EDGE('',*,*,#2240,.F.);
#3047=ORIENTED_EDGE('',*,*,#2241,.F.);
#3048=ORIENTED_EDGE('',*,*,#2242,.T.);
#3049=ORIENTED_EDGE('',*,*,#2241,.T.);
#3050=ORIENTED_EDGE('',*,*,#2243,.F.);
#3051=ORIENTED_EDGE('',*,*,#2244,.F.);
#3052=ORIENTED_EDGE('',*,*,#2245,.T.);
#3053=ORIENTED_EDGE('',*,*,#2244,.T.);
#3054=ORIENTED_EDGE('',*,*,#2246,.F.);
#3055=ORIENTED_EDGE('',*,*,#2247,.F.);
#3056=ORIENTED_EDGE('',*,*,#2248,.T.);
#3057=ORIENTED_EDGE('',*,*,#2247,.T.);
#3058=ORIENTED_EDGE('',*,*,#2249,.F.);
#3059=ORIENTED_EDGE('',*,*,#2250,.F.);
#3060=ORIENTED_EDGE('',*,*,#2251,.T.);
#3061=ORIENTED_EDGE('',*,*,#2250,.T.);
#3062=ORIENTED_EDGE('',*,*,#2252,.F.);
#3063=ORIENTED_EDGE('',*,*,#2253,.F.);
#3064=ORIENTED_EDGE('',*,*,#2254,.T.);
#3065=ORIENTED_EDGE('',*,*,#2253,.T.);
#3066=ORIENTED_EDGE('',*,*,#2255,.F.);
#3067=ORIENTED_EDGE('',*,*,#2256,.F.);
#3068=ORIENTED_EDGE('',*,*,#2257,.T.);
#3069=ORIENTED_EDGE('',*,*,#2256,.T.);
#3070=ORIENTED_EDGE('',*,*,#2258,.F.);
#3071=ORIENTED_EDGE('',*,*,#2259,.F.);
#3072=ORIENTED_EDGE('',*,*,#2260,.T.);
#3073=ORIENTED_EDGE('',*,*,#2259,.T.);
#3074=ORIENTED_EDGE('',*,*,#2261,.F.);
#3075=ORIENTED_EDGE('',*,*,#2262,.F.);
#3076=ORIENTED_EDGE('',*,*,#2263,.T.);
#3077=ORIENTED_EDGE('',*,*,#2262,.T.);
#3078=ORIENTED_EDGE('',*,*,#2264,.F.);
#3079=ORIENTED_EDGE('',*,*,#2265,.F.);
#3080=ORIENTED_EDGE('',*,*,#2266,.T.);
#3081=ORIENTED_EDGE('',*,*,#2265,.T.);
#3082=ORIENTED_EDGE('',*,*,#2267,.F.);
#3083=ORIENTED_EDGE('',*,*,#2239,.F.);
#3084=ORIENTED_EDGE('',*,*,#2267,.T.);
#3085=ORIENTED_EDGE('',*,*,#2264,.T.);
#3086=ORIENTED_EDGE('',*,*,#2261,.T.);
#3087=ORIENTED_EDGE('',*,*,#2258,.T.);
#3088=ORIENTED_EDGE('',*,*,#2255,.T.);
#3089=ORIENTED_EDGE('',*,*,#2252,.T.);
#3090=ORIENTED_EDGE('',*,*,#2249,.T.);
#3091=ORIENTED_EDGE('',*,*,#2246,.T.);
#3092=ORIENTED_EDGE('',*,*,#2243,.T.);
#3093=ORIENTED_EDGE('',*,*,#2240,.T.);
#3094=ORIENTED_EDGE('',*,*,#2235,.T.);
#3095=ORIENTED_EDGE('',*,*,#2232,.T.);
#3096=ORIENTED_EDGE('',*,*,#2229,.T.);
#3097=ORIENTED_EDGE('',*,*,#2226,.T.);
#3098=ORIENTED_EDGE('',*,*,#2266,.F.);
#3099=ORIENTED_EDGE('',*,*,#2238,.F.);
#3100=ORIENTED_EDGE('',*,*,#2242,.F.);
#3101=ORIENTED_EDGE('',*,*,#2245,.F.);
#3102=ORIENTED_EDGE('',*,*,#2248,.F.);
#3103=ORIENTED_EDGE('',*,*,#2251,.F.);
#3104=ORIENTED_EDGE('',*,*,#2254,.F.);
#3105=ORIENTED_EDGE('',*,*,#2257,.F.);
#3106=ORIENTED_EDGE('',*,*,#2260,.F.);
#3107=ORIENTED_EDGE('',*,*,#2263,.F.);
#3108=ORIENTED_EDGE('',*,*,#2237,.F.);
#3109=ORIENTED_EDGE('',*,*,#2234,.F.);
#3110=ORIENTED_EDGE('',*,*,#2231,.F.);
#3111=ORIENTED_EDGE('',*,*,#2228,.F.);
#3112=ORIENTED_EDGE('',*,*,#2268,.T.);
#3113=ORIENTED_EDGE('',*,*,#2269,.T.);
#3114=ORIENTED_EDGE('',*,*,#2270,.F.);
#3115=ORIENTED_EDGE('',*,*,#2269,.F.);
#3116=ORIENTED_EDGE('',*,*,#2271,.T.);
#3117=ORIENTED_EDGE('',*,*,#2272,.T.);
#3118=ORIENTED_EDGE('',*,*,#2273,.F.);
#3119=ORIENTED_EDGE('',*,*,#2272,.F.);
#3120=ORIENTED_EDGE('',*,*,#2274,.T.);
#3121=ORIENTED_EDGE('',*,*,#2275,.T.);
#3122=ORIENTED_EDGE('',*,*,#2276,.F.);
#3123=ORIENTED_EDGE('',*,*,#2275,.F.);
#3124=ORIENTED_EDGE('',*,*,#2277,.T.);
#3125=ORIENTED_EDGE('',*,*,#2278,.T.);
#3126=ORIENTED_EDGE('',*,*,#2279,.F.);
#3127=ORIENTED_EDGE('',*,*,#2278,.F.);
#3128=ORIENTED_EDGE('',*,*,#2280,.F.);
#3129=ORIENTED_EDGE('',*,*,#2281,.T.);
#3130=ORIENTED_EDGE('',*,*,#2282,.T.);
#3131=ORIENTED_EDGE('',*,*,#2283,.F.);
#3132=ORIENTED_EDGE('',*,*,#2284,.F.);
#3133=ORIENTED_EDGE('',*,*,#2285,.T.);
#3134=ORIENTED_EDGE('',*,*,#2286,.T.);
#3135=ORIENTED_EDGE('',*,*,#2281,.F.);
#3136=ORIENTED_EDGE('',*,*,#2287,.F.);
#3137=ORIENTED_EDGE('',*,*,#2288,.T.);
#3138=ORIENTED_EDGE('',*,*,#2289,.T.);
#3139=ORIENTED_EDGE('',*,*,#2285,.F.);
#3140=ORIENTED_EDGE('',*,*,#2290,.F.);
#3141=ORIENTED_EDGE('',*,*,#2291,.T.);
#3142=ORIENTED_EDGE('',*,*,#2292,.T.);
#3143=ORIENTED_EDGE('',*,*,#2288,.F.);
#3144=ORIENTED_EDGE('',*,*,#2293,.F.);
#3145=ORIENTED_EDGE('',*,*,#2294,.T.);
#3146=ORIENTED_EDGE('',*,*,#2295,.T.);
#3147=ORIENTED_EDGE('',*,*,#2291,.F.);
#3148=ORIENTED_EDGE('',*,*,#2296,.F.);
#3149=ORIENTED_EDGE('',*,*,#2297,.T.);
#3150=ORIENTED_EDGE('',*,*,#2298,.T.);
#3151=ORIENTED_EDGE('',*,*,#2294,.F.);
#3152=ORIENTED_EDGE('',*,*,#2299,.F.);
#3153=ORIENTED_EDGE('',*,*,#2300,.T.);
#3154=ORIENTED_EDGE('',*,*,#2301,.T.);
#3155=ORIENTED_EDGE('',*,*,#2297,.F.);
#3156=ORIENTED_EDGE('',*,*,#2302,.F.);
#3157=ORIENTED_EDGE('',*,*,#2303,.T.);
#3158=ORIENTED_EDGE('',*,*,#2304,.T.);
#3159=ORIENTED_EDGE('',*,*,#2300,.F.);
#3160=ORIENTED_EDGE('',*,*,#2305,.F.);
#3161=ORIENTED_EDGE('',*,*,#2306,.T.);
#3162=ORIENTED_EDGE('',*,*,#2307,.T.);
#3163=ORIENTED_EDGE('',*,*,#2303,.F.);
#3164=ORIENTED_EDGE('',*,*,#2308,.F.);
#3165=ORIENTED_EDGE('',*,*,#2283,.T.);
#3166=ORIENTED_EDGE('',*,*,#2309,.T.);
#3167=ORIENTED_EDGE('',*,*,#2306,.F.);
#3168=ORIENTED_EDGE('',*,*,#2309,.F.);
#3169=ORIENTED_EDGE('',*,*,#2282,.F.);
#3170=ORIENTED_EDGE('',*,*,#2286,.F.);
#3171=ORIENTED_EDGE('',*,*,#2289,.F.);
#3172=ORIENTED_EDGE('',*,*,#2292,.F.);
#3173=ORIENTED_EDGE('',*,*,#2295,.F.);
#3174=ORIENTED_EDGE('',*,*,#2298,.F.);
#3175=ORIENTED_EDGE('',*,*,#2301,.F.);
#3176=ORIENTED_EDGE('',*,*,#2304,.F.);
#3177=ORIENTED_EDGE('',*,*,#2307,.F.);
#3178=ORIENTED_EDGE('',*,*,#2277,.F.);
#3179=ORIENTED_EDGE('',*,*,#2274,.F.);
#3180=ORIENTED_EDGE('',*,*,#2271,.F.);
#3181=ORIENTED_EDGE('',*,*,#2268,.F.);
#3182=ORIENTED_EDGE('',*,*,#2308,.T.);
#3183=ORIENTED_EDGE('',*,*,#2305,.T.);
#3184=ORIENTED_EDGE('',*,*,#2302,.T.);
#3185=ORIENTED_EDGE('',*,*,#2299,.T.);
#3186=ORIENTED_EDGE('',*,*,#2296,.T.);
#3187=ORIENTED_EDGE('',*,*,#2293,.T.);
#3188=ORIENTED_EDGE('',*,*,#2290,.T.);
#3189=ORIENTED_EDGE('',*,*,#2287,.T.);
#3190=ORIENTED_EDGE('',*,*,#2284,.T.);
#3191=ORIENTED_EDGE('',*,*,#2280,.T.);
#3192=ORIENTED_EDGE('',*,*,#2279,.T.);
#3193=ORIENTED_EDGE('',*,*,#2276,.T.);
#3194=ORIENTED_EDGE('',*,*,#2273,.T.);
#3195=ORIENTED_EDGE('',*,*,#2270,.T.);
#3196=ORIENTED_EDGE('',*,*,#2310,.T.);
#3197=ORIENTED_EDGE('',*,*,#2311,.T.);
#3198=ORIENTED_EDGE('',*,*,#2312,.F.);
#3199=ORIENTED_EDGE('',*,*,#2311,.F.);
#3200=ORIENTED_EDGE('',*,*,#2313,.T.);
#3201=ORIENTED_EDGE('',*,*,#2314,.T.);
#3202=ORIENTED_EDGE('',*,*,#2315,.F.);
#3203=ORIENTED_EDGE('',*,*,#2314,.F.);
#3204=ORIENTED_EDGE('',*,*,#2316,.T.);
#3205=ORIENTED_EDGE('',*,*,#2317,.T.);
#3206=ORIENTED_EDGE('',*,*,#2318,.F.);
#3207=ORIENTED_EDGE('',*,*,#2317,.F.);
#3208=ORIENTED_EDGE('',*,*,#2319,.T.);
#3209=ORIENTED_EDGE('',*,*,#2320,.T.);
#3210=ORIENTED_EDGE('',*,*,#2321,.F.);
#3211=ORIENTED_EDGE('',*,*,#2320,.F.);
#3212=ORIENTED_EDGE('',*,*,#2322,.F.);
#3213=ORIENTED_EDGE('',*,*,#2323,.T.);
#3214=ORIENTED_EDGE('',*,*,#2324,.T.);
#3215=ORIENTED_EDGE('',*,*,#2325,.F.);
#3216=ORIENTED_EDGE('',*,*,#2326,.F.);
#3217=ORIENTED_EDGE('',*,*,#2327,.T.);
#3218=ORIENTED_EDGE('',*,*,#2328,.T.);
#3219=ORIENTED_EDGE('',*,*,#2323,.F.);
#3220=ORIENTED_EDGE('',*,*,#2329,.F.);
#3221=ORIENTED_EDGE('',*,*,#2330,.T.);
#3222=ORIENTED_EDGE('',*,*,#2331,.T.);
#3223=ORIENTED_EDGE('',*,*,#2327,.F.);
#3224=ORIENTED_EDGE('',*,*,#2332,.F.);
#3225=ORIENTED_EDGE('',*,*,#2333,.T.);
#3226=ORIENTED_EDGE('',*,*,#2334,.T.);
#3227=ORIENTED_EDGE('',*,*,#2330,.F.);
#3228=ORIENTED_EDGE('',*,*,#2335,.F.);
#3229=ORIENTED_EDGE('',*,*,#2336,.T.);
#3230=ORIENTED_EDGE('',*,*,#2337,.T.);
#3231=ORIENTED_EDGE('',*,*,#2333,.F.);
#3232=ORIENTED_EDGE('',*,*,#2338,.F.);
#3233=ORIENTED_EDGE('',*,*,#2339,.T.);
#3234=ORIENTED_EDGE('',*,*,#2340,.T.);
#3235=ORIENTED_EDGE('',*,*,#2336,.F.);
#3236=ORIENTED_EDGE('',*,*,#2341,.F.);
#3237=ORIENTED_EDGE('',*,*,#2342,.T.);
#3238=ORIENTED_EDGE('',*,*,#2343,.T.);
#3239=ORIENTED_EDGE('',*,*,#2339,.F.);
#3240=ORIENTED_EDGE('',*,*,#2344,.F.);
#3241=ORIENTED_EDGE('',*,*,#2345,.T.);
#3242=ORIENTED_EDGE('',*,*,#2346,.T.);
#3243=ORIENTED_EDGE('',*,*,#2342,.F.);
#3244=ORIENTED_EDGE('',*,*,#2347,.F.);
#3245=ORIENTED_EDGE('',*,*,#2348,.T.);
#3246=ORIENTED_EDGE('',*,*,#2349,.T.);
#3247=ORIENTED_EDGE('',*,*,#2345,.F.);
#3248=ORIENTED_EDGE('',*,*,#2350,.F.);
#3249=ORIENTED_EDGE('',*,*,#2325,.T.);
#3250=ORIENTED_EDGE('',*,*,#2351,.T.);
#3251=ORIENTED_EDGE('',*,*,#2348,.F.);
#3252=ORIENTED_EDGE('',*,*,#2351,.F.);
#3253=ORIENTED_EDGE('',*,*,#2324,.F.);
#3254=ORIENTED_EDGE('',*,*,#2328,.F.);
#3255=ORIENTED_EDGE('',*,*,#2331,.F.);
#3256=ORIENTED_EDGE('',*,*,#2334,.F.);
#3257=ORIENTED_EDGE('',*,*,#2337,.F.);
#3258=ORIENTED_EDGE('',*,*,#2340,.F.);
#3259=ORIENTED_EDGE('',*,*,#2343,.F.);
#3260=ORIENTED_EDGE('',*,*,#2346,.F.);
#3261=ORIENTED_EDGE('',*,*,#2349,.F.);
#3262=ORIENTED_EDGE('',*,*,#2319,.F.);
#3263=ORIENTED_EDGE('',*,*,#2316,.F.);
#3264=ORIENTED_EDGE('',*,*,#2313,.F.);
#3265=ORIENTED_EDGE('',*,*,#2310,.F.);
#3266=ORIENTED_EDGE('',*,*,#2350,.T.);
#3267=ORIENTED_EDGE('',*,*,#2347,.T.);
#3268=ORIENTED_EDGE('',*,*,#2344,.T.);
#3269=ORIENTED_EDGE('',*,*,#2341,.T.);
#3270=ORIENTED_EDGE('',*,*,#2338,.T.);
#3271=ORIENTED_EDGE('',*,*,#2335,.T.);
#3272=ORIENTED_EDGE('',*,*,#2332,.T.);
#3273=ORIENTED_EDGE('',*,*,#2329,.T.);
#3274=ORIENTED_EDGE('',*,*,#2326,.T.);
#3275=ORIENTED_EDGE('',*,*,#2322,.T.);
#3276=ORIENTED_EDGE('',*,*,#2321,.T.);
#3277=ORIENTED_EDGE('',*,*,#2318,.T.);
#3278=ORIENTED_EDGE('',*,*,#2315,.T.);
#3279=ORIENTED_EDGE('',*,*,#2312,.T.);
#3280=ORIENTED_EDGE('',*,*,#2352,.F.);
#3281=ORIENTED_EDGE('',*,*,#2353,.T.);
#3282=ORIENTED_EDGE('',*,*,#2354,.T.);
#3283=ORIENTED_EDGE('',*,*,#2353,.F.);
#3284=ORIENTED_EDGE('',*,*,#2355,.F.);
#3285=ORIENTED_EDGE('',*,*,#2356,.T.);
#3286=ORIENTED_EDGE('',*,*,#2357,.T.);
#3287=ORIENTED_EDGE('',*,*,#2356,.F.);
#3288=ORIENTED_EDGE('',*,*,#2358,.F.);
#3289=ORIENTED_EDGE('',*,*,#2359,.T.);
#3290=ORIENTED_EDGE('',*,*,#2360,.T.);
#3291=ORIENTED_EDGE('',*,*,#2359,.F.);
#3292=ORIENTED_EDGE('',*,*,#2361,.F.);
#3293=ORIENTED_EDGE('',*,*,#2362,.T.);
#3294=ORIENTED_EDGE('',*,*,#2363,.T.);
#3295=ORIENTED_EDGE('',*,*,#2362,.F.);
#3296=ORIENTED_EDGE('',*,*,#2364,.T.);
#3297=ORIENTED_EDGE('',*,*,#2365,.T.);
#3298=ORIENTED_EDGE('',*,*,#2366,.F.);
#3299=ORIENTED_EDGE('',*,*,#2367,.F.);
#3300=ORIENTED_EDGE('',*,*,#2368,.T.);
#3301=ORIENTED_EDGE('',*,*,#2367,.T.);
#3302=ORIENTED_EDGE('',*,*,#2369,.F.);
#3303=ORIENTED_EDGE('',*,*,#2370,.F.);
#3304=ORIENTED_EDGE('',*,*,#2371,.T.);
#3305=ORIENTED_EDGE('',*,*,#2370,.T.);
#3306=ORIENTED_EDGE('',*,*,#2372,.F.);
#3307=ORIENTED_EDGE('',*,*,#2373,.F.);
#3308=ORIENTED_EDGE('',*,*,#2374,.T.);
#3309=ORIENTED_EDGE('',*,*,#2373,.T.);
#3310=ORIENTED_EDGE('',*,*,#2375,.F.);
#3311=ORIENTED_EDGE('',*,*,#2376,.F.);
#3312=ORIENTED_EDGE('',*,*,#2377,.T.);
#3313=ORIENTED_EDGE('',*,*,#2376,.T.);
#3314=ORIENTED_EDGE('',*,*,#2378,.F.);
#3315=ORIENTED_EDGE('',*,*,#2379,.F.);
#3316=ORIENTED_EDGE('',*,*,#2380,.T.);
#3317=ORIENTED_EDGE('',*,*,#2379,.T.);
#3318=ORIENTED_EDGE('',*,*,#2381,.F.);
#3319=ORIENTED_EDGE('',*,*,#2382,.F.);
#3320=ORIENTED_EDGE('',*,*,#2383,.T.);
#3321=ORIENTED_EDGE('',*,*,#2382,.T.);
#3322=ORIENTED_EDGE('',*,*,#2384,.F.);
#3323=ORIENTED_EDGE('',*,*,#2385,.F.);
#3324=ORIENTED_EDGE('',*,*,#2386,.T.);
#3325=ORIENTED_EDGE('',*,*,#2385,.T.);
#3326=ORIENTED_EDGE('',*,*,#2387,.F.);
#3327=ORIENTED_EDGE('',*,*,#2388,.F.);
#3328=ORIENTED_EDGE('',*,*,#2389,.T.);
#3329=ORIENTED_EDGE('',*,*,#2388,.T.);
#3330=ORIENTED_EDGE('',*,*,#2390,.F.);
#3331=ORIENTED_EDGE('',*,*,#2391,.F.);
#3332=ORIENTED_EDGE('',*,*,#2392,.T.);
#3333=ORIENTED_EDGE('',*,*,#2391,.T.);
#3334=ORIENTED_EDGE('',*,*,#2393,.F.);
#3335=ORIENTED_EDGE('',*,*,#2365,.F.);
#3336=ORIENTED_EDGE('',*,*,#2393,.T.);
#3337=ORIENTED_EDGE('',*,*,#2390,.T.);
#3338=ORIENTED_EDGE('',*,*,#2387,.T.);
#3339=ORIENTED_EDGE('',*,*,#2384,.T.);
#3340=ORIENTED_EDGE('',*,*,#2381,.T.);
#3341=ORIENTED_EDGE('',*,*,#2378,.T.);
#3342=ORIENTED_EDGE('',*,*,#2375,.T.);
#3343=ORIENTED_EDGE('',*,*,#2372,.T.);
#3344=ORIENTED_EDGE('',*,*,#2369,.T.);
#3345=ORIENTED_EDGE('',*,*,#2366,.T.);
#3346=ORIENTED_EDGE('',*,*,#2361,.T.);
#3347=ORIENTED_EDGE('',*,*,#2358,.T.);
#3348=ORIENTED_EDGE('',*,*,#2355,.T.);
#3349=ORIENTED_EDGE('',*,*,#2352,.T.);
#3350=ORIENTED_EDGE('',*,*,#2392,.F.);
#3351=ORIENTED_EDGE('',*,*,#2364,.F.);
#3352=ORIENTED_EDGE('',*,*,#2368,.F.);
#3353=ORIENTED_EDGE('',*,*,#2371,.F.);
#3354=ORIENTED_EDGE('',*,*,#2374,.F.);
#3355=ORIENTED_EDGE('',*,*,#2377,.F.);
#3356=ORIENTED_EDGE('',*,*,#2380,.F.);
#3357=ORIENTED_EDGE('',*,*,#2383,.F.);
#3358=ORIENTED_EDGE('',*,*,#2386,.F.);
#3359=ORIENTED_EDGE('',*,*,#2389,.F.);
#3360=ORIENTED_EDGE('',*,*,#2363,.F.);
#3361=ORIENTED_EDGE('',*,*,#2360,.F.);
#3362=ORIENTED_EDGE('',*,*,#2357,.F.);
#3363=ORIENTED_EDGE('',*,*,#2354,.F.);
#3364=CYLINDRICAL_SURFACE('',#3728,11.);
#3365=CYLINDRICAL_SURFACE('',#3731,11.);
#3366=CYLINDRICAL_SURFACE('',#3735,7.61489399011346);
#3367=CYLINDRICAL_SURFACE('',#3740,7.61489399011346);
#3368=CYLINDRICAL_SURFACE('',#3745,7.61489399011346);
#3369=CYLINDRICAL_SURFACE('',#3756,7.61489399011346);
#3370=CYLINDRICAL_SURFACE('',#3761,7.61489399011346);
#3371=CYLINDRICAL_SURFACE('',#3766,7.61489399011346);
#3372=CYLINDRICAL_SURFACE('',#3795,12.5);
#3373=CYLINDRICAL_SURFACE('',#3805,7.5);
#3374=CYLINDRICAL_SURFACE('',#3807,11.5112);
#3375=CYLINDRICAL_SURFACE('',#3835,10.);
#3376=CYLINDRICAL_SURFACE('',#3837,10.);
#3377=CYLINDRICAL_SURFACE('',#3839,10.);
#3378=CYLINDRICAL_SURFACE('',#3841,10.);
#3379=CYLINDRICAL_SURFACE('',#3857,5.);
#3380=CYLINDRICAL_SURFACE('',#3865,5.);
#3381=CYLINDRICAL_SURFACE('',#3867,5.);
#3382=CYLINDRICAL_SURFACE('',#3870,5.);
#3383=CYLINDRICAL_SURFACE('',#3876,7.5);
#3384=CYLINDRICAL_SURFACE('',#3880,10.88225);
#3385=CYLINDRICAL_SURFACE('',#3886,11.);
#3386=CYLINDRICAL_SURFACE('',#3908,31.837899857748);
#3387=CYLINDRICAL_SURFACE('',#3916,13.946575006305);
#3388=CYLINDRICAL_SURFACE('',#3929,36.8878705819456);
#3389=CYLINDRICAL_SURFACE('',#3933,1.99999999999999);
#3390=CYLINDRICAL_SURFACE('',#3936,1.99999999999999);
#3391=CYLINDRICAL_SURFACE('',#3939,1.99999999999999);
#3392=CYLINDRICAL_SURFACE('',#3942,1.99999999999999);
#3393=CYLINDRICAL_SURFACE('',#3958,1.99999999999999);
#3394=CYLINDRICAL_SURFACE('',#3961,1.99999999999999);
#3395=CYLINDRICAL_SURFACE('',#3964,1.99999999999999);
#3396=CYLINDRICAL_SURFACE('',#3967,1.99999999999999);
#3397=CYLINDRICAL_SURFACE('',#3983,1.99999999999999);
#3398=CYLINDRICAL_SURFACE('',#3986,1.99999999999999);
#3399=CYLINDRICAL_SURFACE('',#3989,1.99999999999999);
#3400=CYLINDRICAL_SURFACE('',#3992,1.99999999999999);
#3401=CYLINDRICAL_SURFACE('',#4008,1.99999999999999);
#3402=CYLINDRICAL_SURFACE('',#4011,1.99999999999999);
#3403=CYLINDRICAL_SURFACE('',#4014,1.99999999999999);
#3404=CYLINDRICAL_SURFACE('',#4017,1.99999999999999);
#3405=ADVANCED_FACE('',(#298),#3364,.F.);
#3406=ADVANCED_FACE('',(#299),#3365,.F.);
#3407=ADVANCED_FACE('',(#300),#158,.T.);
#3408=ADVANCED_FACE('',(#301),#3366,.F.);
#3409=ADVANCED_FACE('',(#302),#159,.T.);
#3410=ADVANCED_FACE('',(#303),#160,.T.);
#3411=ADVANCED_FACE('',(#304),#3367,.F.);
#3412=ADVANCED_FACE('',(#305),#161,.T.);
#3413=ADVANCED_FACE('',(#306),#162,.T.);
#3414=ADVANCED_FACE('',(#307),#3368,.F.);
#3415=ADVANCED_FACE('',(#308),#163,.T.);
#3416=ADVANCED_FACE('',(#309),#164,.T.);
#3417=ADVANCED_FACE('',(#310),#165,.T.);
#3418=ADVANCED_FACE('',(#311),#166,.T.);
#3419=ADVANCED_FACE('',(#312),#167,.T.);
#3420=ADVANCED_FACE('',(#313),#168,.T.);
#3421=ADVANCED_FACE('',(#314),#169,.F.);
#3422=ADVANCED_FACE('',(#315),#170,.F.);
#3423=ADVANCED_FACE('',(#316),#3369,.F.);
#3424=ADVANCED_FACE('',(#317),#171,.F.);
#3425=ADVANCED_FACE('',(#318),#172,.F.);
#3426=ADVANCED_FACE('',(#319),#3370,.F.);
#3427=ADVANCED_FACE('',(#320),#173,.F.);
#3428=ADVANCED_FACE('',(#321),#174,.F.);
#3429=ADVANCED_FACE('',(#322),#3371,.F.);
#3430=ADVANCED_FACE('',(#323),#175,.T.);
#3431=ADVANCED_FACE('',(#324),#176,.T.);
#3432=ADVANCED_FACE('',(#325),#177,.T.);
#3433=ADVANCED_FACE('',(#326),#178,.T.);
#3434=ADVANCED_FACE('',(#327),#179,.T.);
#3435=ADVANCED_FACE('',(#328,#106),#180,.F.);
#3436=ADVANCED_FACE('',(#329),#181,.T.);
#3437=ADVANCED_FACE('',(#330),#182,.T.);
#3438=ADVANCED_FACE('',(#331),#183,.T.);
#3439=ADVANCED_FACE('',(#332,#107),#184,.T.);
#3440=ADVANCED_FACE('',(#333,#108),#185,.F.);
#3441=ADVANCED_FACE('',(#334),#186,.T.);
#3442=ADVANCED_FACE('',(#335),#187,.T.);
#3443=ADVANCED_FACE('',(#336),#188,.T.);
#3444=ADVANCED_FACE('',(#337,#109),#189,.T.);
#3445=ADVANCED_FACE('',(#338),#190,.T.);
#3446=ADVANCED_FACE('',(#339),#191,.T.);
#3447=ADVANCED_FACE('',(#340),#192,.T.);
#3448=ADVANCED_FACE('',(#341),#193,.T.);
#3449=ADVANCED_FACE('',(#342,#110),#194,.T.);
#3450=ADVANCED_FACE('',(#343),#55,.T.);
#3451=ADVANCED_FACE('',(#344),#3372,.T.);
#3452=ADVANCED_FACE('',(#345,#111),#195,.T.);
#3453=ADVANCED_FACE('',(#346),#56,.T.);
#3454=ADVANCED_FACE('',(#347,#112),#196,.F.);
#3455=ADVANCED_FACE('',(#348),#3373,.F.);
#3456=ADVANCED_FACE('',(#349),#3374,.F.);
#3457=ADVANCED_FACE('',(#350,#113),#197,.T.);
#3458=ADVANCED_FACE('',(#351,#114),#198,.T.);
#3459=ADVANCED_FACE('',(#352),#199,.T.);
#3460=ADVANCED_FACE('',(#353),#200,.T.);
#3461=ADVANCED_FACE('',(#354),#201,.T.);
#3462=ADVANCED_FACE('',(#355),#202,.T.);
#3463=ADVANCED_FACE('',(#356),#203,.T.);
#3464=ADVANCED_FACE('',(#357),#204,.T.);
#3465=ADVANCED_FACE('',(#358),#205,.T.);
#3466=ADVANCED_FACE('',(#359),#206,.T.);
#3467=ADVANCED_FACE('',(#360),#207,.T.);
#3468=ADVANCED_FACE('',(#361),#208,.T.);
#3469=ADVANCED_FACE('',(#362),#209,.T.);
#3470=ADVANCED_FACE('',(#363),#3375,.F.);
#3471=ADVANCED_FACE('',(#364),#3376,.F.);
#3472=ADVANCED_FACE('',(#365),#3377,.F.);
#3473=ADVANCED_FACE('',(#366),#3378,.F.);
#3474=ADVANCED_FACE('',(#367),#210,.F.);
#3475=ADVANCED_FACE('',(#368),#211,.F.);
#3476=ADVANCED_FACE('',(#369),#212,.F.);
#3477=ADVANCED_FACE('',(#370),#213,.F.);
#3478=ADVANCED_FACE('',(#371),#214,.F.);
#3479=ADVANCED_FACE('',(#372),#215,.F.);
#3480=ADVANCED_FACE('',(#373),#216,.T.);
#3481=ADVANCED_FACE('',(#374),#217,.T.);
#3482=ADVANCED_FACE('',(#375),#218,.T.);
#3483=ADVANCED_FACE('',(#376,#115,#116,#117,#118),#219,.T.);
#3484=ADVANCED_FACE('',(#377),#220,.T.);
#3485=ADVANCED_FACE('',(#378),#221,.T.);
#3486=ADVANCED_FACE('',(#379),#222,.T.);
#3487=ADVANCED_FACE('',(#380),#3379,.T.);
#3488=ADVANCED_FACE('',(#381),#223,.F.);
#3489=ADVANCED_FACE('',(#382),#224,.T.);
#3490=ADVANCED_FACE('',(#383),#3380,.T.);
#3491=ADVANCED_FACE('',(#384),#3381,.T.);
#3492=ADVANCED_FACE('',(#385),#225,.T.);
#3493=ADVANCED_FACE('',(#386),#3382,.T.);
#3494=ADVANCED_FACE('',(#387),#226,.T.);
#3495=ADVANCED_FACE('',(#388),#227,.T.);
#3496=ADVANCED_FACE('',(#389),#228,.T.);
#3497=ADVANCED_FACE('',(#390),#3383,.T.);
#3498=ADVANCED_FACE('',(#391),#229,.T.);
#3499=ADVANCED_FACE('',(#392),#3384,.T.);
#3500=ADVANCED_FACE('',(#393,#119),#230,.T.);
#3501=ADVANCED_FACE('',(#394),#231,.F.);
#3502=ADVANCED_FACE('',(#395),#3385,.F.);
#3503=ADVANCED_FACE('',(#396),#232,.F.);
#3504=ADVANCED_FACE('',(#397),#233,.F.);
#3505=ADVANCED_FACE('',(#398,#120),#234,.F.);
#3506=ADVANCED_FACE('',(#399),#235,.F.);
#3507=ADVANCED_FACE('',(#400),#236,.T.);
#3508=ADVANCED_FACE('',(#401,#121),#237,.T.);
#3509=ADVANCED_FACE('',(#402,#122),#238,.F.);
#3510=ADVANCED_FACE('',(#403),#239,.T.);
#3511=ADVANCED_FACE('',(#404,#123),#240,.T.);
#3512=ADVANCED_FACE('',(#405),#241,.T.);
#3513=ADVANCED_FACE('',(#406),#242,.T.);
#3514=ADVANCED_FACE('',(#407),#243,.T.);
#3515=ADVANCED_FACE('',(#408),#244,.T.);
#3516=ADVANCED_FACE('',(#409),#245,.T.);
#3517=ADVANCED_FACE('',(#410),#57,.F.);
#3518=ADVANCED_FACE('',(#411),#3386,.T.);
#3519=ADVANCED_FACE('',(#412,#124),#246,.T.);
#3520=ADVANCED_FACE('',(#413),#58,.F.);
#3521=ADVANCED_FACE('',(#414),#3387,.T.);
#3522=ADVANCED_FACE('',(#415,#125),#247,.T.);
#3523=ADVANCED_FACE('',(#416),#59,.T.);
#3524=ADVANCED_FACE('',(#417),#248,.T.);
#3525=ADVANCED_FACE('',(#418),#60,.T.);
#3526=ADVANCED_FACE('',(#419),#61,.T.);
#3527=ADVANCED_FACE('',(#420),#3388,.T.);
#3528=ADVANCED_FACE('',(#421),#249,.T.);
#3529=ADVANCED_FACE('',(#422),#3389,.F.);
#3530=ADVANCED_FACE('',(#423),#3390,.F.);
#3531=ADVANCED_FACE('',(#424),#3391,.F.);
#3532=ADVANCED_FACE('',(#425),#3392,.F.);
#3533=ADVANCED_FACE('',(#426),#250,.T.);
#3534=ADVANCED_FACE('',(#427),#251,.T.);
#3535=ADVANCED_FACE('',(#428),#252,.T.);
#3536=ADVANCED_FACE('',(#429),#253,.T.);
#3537=ADVANCED_FACE('',(#430),#254,.T.);
#3538=ADVANCED_FACE('',(#431),#255,.T.);
#3539=ADVANCED_FACE('',(#432),#256,.T.);
#3540=ADVANCED_FACE('',(#433),#257,.T.);
#3541=ADVANCED_FACE('',(#434),#258,.T.);
#3542=ADVANCED_FACE('',(#435),#259,.T.);
#3543=ADVANCED_FACE('',(#436,#126,#127,#128,#129),#260,.T.);
#3544=ADVANCED_FACE('',(#437,#130,#131,#132,#133),#261,.F.);
#3545=ADVANCED_FACE('',(#438),#3393,.F.);
#3546=ADVANCED_FACE('',(#439),#3394,.F.);
#3547=ADVANCED_FACE('',(#440),#3395,.F.);
#3548=ADVANCED_FACE('',(#441),#3396,.F.);
#3549=ADVANCED_FACE('',(#442),#262,.F.);
#3550=ADVANCED_FACE('',(#443),#263,.F.);
#3551=ADVANCED_FACE('',(#444),#264,.F.);
#3552=ADVANCED_FACE('',(#445),#265,.F.);
#3553=ADVANCED_FACE('',(#446),#266,.F.);
#3554=ADVANCED_FACE('',(#447),#267,.F.);
#3555=ADVANCED_FACE('',(#448),#268,.F.);
#3556=ADVANCED_FACE('',(#449),#269,.F.);
#3557=ADVANCED_FACE('',(#450),#270,.F.);
#3558=ADVANCED_FACE('',(#451),#271,.F.);
#3559=ADVANCED_FACE('',(#452,#134,#135,#136,#137),#272,.F.);
#3560=ADVANCED_FACE('',(#453,#138,#139,#140,#141),#273,.T.);
#3561=ADVANCED_FACE('',(#454),#3397,.F.);
#3562=ADVANCED_FACE('',(#455),#3398,.F.);
#3563=ADVANCED_FACE('',(#456),#3399,.F.);
#3564=ADVANCED_FACE('',(#457),#3400,.F.);
#3565=ADVANCED_FACE('',(#458),#274,.F.);
#3566=ADVANCED_FACE('',(#459),#275,.F.);
#3567=ADVANCED_FACE('',(#460),#276,.F.);
#3568=ADVANCED_FACE('',(#461),#277,.F.);
#3569=ADVANCED_FACE('',(#462),#278,.F.);
#3570=ADVANCED_FACE('',(#463),#279,.F.);
#3571=ADVANCED_FACE('',(#464),#280,.F.);
#3572=ADVANCED_FACE('',(#465),#281,.F.);
#3573=ADVANCED_FACE('',(#466),#282,.F.);
#3574=ADVANCED_FACE('',(#467),#283,.F.);
#3575=ADVANCED_FACE('',(#468,#142,#143,#144,#145),#284,.F.);
#3576=ADVANCED_FACE('',(#469,#146,#147,#148,#149),#285,.T.);
#3577=ADVANCED_FACE('',(#470),#3401,.F.);
#3578=ADVANCED_FACE('',(#471),#3402,.F.);
#3579=ADVANCED_FACE('',(#472),#3403,.F.);
#3580=ADVANCED_FACE('',(#473),#3404,.F.);
#3581=ADVANCED_FACE('',(#474),#286,.T.);
#3582=ADVANCED_FACE('',(#475),#287,.T.);
#3583=ADVANCED_FACE('',(#476),#288,.T.);
#3584=ADVANCED_FACE('',(#477),#289,.T.);
#3585=ADVANCED_FACE('',(#478),#290,.T.);
#3586=ADVANCED_FACE('',(#479),#291,.T.);
#3587=ADVANCED_FACE('',(#480),#292,.T.);
#3588=ADVANCED_FACE('',(#481),#293,.T.);
#3589=ADVANCED_FACE('',(#482),#294,.T.);
#3590=ADVANCED_FACE('',(#483),#295,.T.);
#3591=ADVANCED_FACE('',(#484,#150,#151,#152,#153),#296,.T.);
#3592=ADVANCED_FACE('',(#485,#154,#155,#156,#157),#297,.F.);
#3593=CLOSED_SHELL('',(#3405,#3406,#3407,#3408,#3409,#3410,#3411,#3412,
#3413,#3414,#3415,#3416,#3417,#3418,#3419,#3420,#3421,#3422,#3423,#3424,
#3425,#3426,#3427,#3428,#3429,#3430,#3431,#3432,#3433,#3434,#3435,#3436,
#3437,#3438,#3439,#3440,#3441,#3442,#3443,#3444,#3445,#3446,#3447,#3448,
#3449));
#3594=CLOSED_SHELL('',(#3450,#3451,#3452,#3453,#3454,#3455));
#3595=CLOSED_SHELL('',(#3456,#3457,#3458,#3459,#3460,#3461,#3462,#3463,
#3464,#3465,#3466,#3467,#3468,#3469,#3470,#3471,#3472,#3473,#3474,#3475,
#3476,#3477,#3478,#3479,#3480,#3481,#3482,#3483,#3484,#3485,#3486));
#3596=CLOSED_SHELL('',(#3487,#3488,#3489,#3490,#3491,#3492,#3493,#3494,
#3495,#3496));
#3597=CLOSED_SHELL('',(#3497,#3498,#3499,#3500,#3501));
#3598=CLOSED_SHELL('',(#3502,#3503,#3504,#3505,#3506,#3507,#3508,#3509,
#3510,#3511,#3512,#3513,#3514,#3515,#3516));
#3599=CLOSED_SHELL('',(#3517,#3518,#3519,#3520,#3521,#3522,#3523,#3524,
#3525,#3526,#3527,#3528));
#3600=CLOSED_SHELL('',(#3529,#3530,#3531,#3532,#3533,#3534,#3535,#3536,
#3537,#3538,#3539,#3540,#3541,#3542,#3543,#3544));
#3601=CLOSED_SHELL('',(#3545,#3546,#3547,#3548,#3549,#3550,#3551,#3552,
#3553,#3554,#3555,#3556,#3557,#3558,#3559,#3560));
#3602=CLOSED_SHELL('',(#3561,#3562,#3563,#3564,#3565,#3566,#3567,#3568,
#3569,#3570,#3571,#3572,#3573,#3574,#3575,#3576));
#3603=CLOSED_SHELL('',(#3577,#3578,#3579,#3580,#3581,#3582,#3583,#3584,
#3585,#3586,#3587,#3588,#3589,#3590,#3591,#3592));
#3604=DERIVED_UNIT_ELEMENT(#3626,1.);
#3605=DERIVED_UNIT_ELEMENT(#6098,-3.);
#3606=DERIVED_UNIT_ELEMENT(#3626,1.);
#3607=DERIVED_UNIT_ELEMENT(#6098,-3.);
#3608=DERIVED_UNIT_ELEMENT(#3626,1.);
#3609=DERIVED_UNIT_ELEMENT(#6098,-3.);
#3610=DERIVED_UNIT_ELEMENT(#3626,1.);
#3611=DERIVED_UNIT_ELEMENT(#6098,-3.);
#3612=DERIVED_UNIT_ELEMENT(#3626,1.);
#3613=DERIVED_UNIT_ELEMENT(#6098,-3.);
#3614=DERIVED_UNIT_ELEMENT(#3626,1.);
#3615=DERIVED_UNIT_ELEMENT(#6098,-3.);
#3616=DERIVED_UNIT_ELEMENT(#3626,1.);
#3617=DERIVED_UNIT_ELEMENT(#6098,-3.);
#3618=DERIVED_UNIT_ELEMENT(#3626,1.);
#3619=DERIVED_UNIT_ELEMENT(#6098,-3.);
#3620=DERIVED_UNIT_ELEMENT(#3626,1.);
#3621=DERIVED_UNIT_ELEMENT(#6098,-3.);
#3622=DERIVED_UNIT_ELEMENT(#3626,1.);
#3623=DERIVED_UNIT_ELEMENT(#6098,-3.);
#3624=DERIVED_UNIT_ELEMENT(#3626,1.);
#3625=DERIVED_UNIT_ELEMENT(#6098,-3.);
#3626=(
MASS_UNIT()
NAMED_UNIT(*)
SI_UNIT(.KILO.,.GRAM.)
);
#3627=DERIVED_UNIT((#3604,#3605));
#3628=DERIVED_UNIT((#3606,#3607));
#3629=DERIVED_UNIT((#3608,#3609));
#3630=DERIVED_UNIT((#3610,#3611));
#3631=DERIVED_UNIT((#3612,#3613));
#3632=DERIVED_UNIT((#3614,#3615));
#3633=DERIVED_UNIT((#3616,#3617));
#3634=DERIVED_UNIT((#3618,#3619));
#3635=DERIVED_UNIT((#3620,#3621));
#3636=DERIVED_UNIT((#3622,#3623));
#3637=DERIVED_UNIT((#3624,#3625));
#3638=MEASURE_REPRESENTATION_ITEM('density measure',
POSITIVE_RATIO_MEASURE(7850.),#3627);
#3639=MEASURE_REPRESENTATION_ITEM('density measure',
POSITIVE_RATIO_MEASURE(7850.),#3628);
#3640=MEASURE_REPRESENTATION_ITEM('density measure',
POSITIVE_RATIO_MEASURE(7850.),#3629);
#3641=MEASURE_REPRESENTATION_ITEM('density measure',
POSITIVE_RATIO_MEASURE(7850.),#3630);
#3642=MEASURE_REPRESENTATION_ITEM('density measure',
POSITIVE_RATIO_MEASURE(7850.),#3631);
#3643=MEASURE_REPRESENTATION_ITEM('density measure',
POSITIVE_RATIO_MEASURE(7850.),#3632);
#3644=MEASURE_REPRESENTATION_ITEM('density measure',
POSITIVE_RATIO_MEASURE(7850.),#3633);
#3645=MEASURE_REPRESENTATION_ITEM('density measure',
POSITIVE_RATIO_MEASURE(7850.),#3634);
#3646=MEASURE_REPRESENTATION_ITEM('density measure',
POSITIVE_RATIO_MEASURE(7850.),#3635);
#3647=MEASURE_REPRESENTATION_ITEM('density measure',
POSITIVE_RATIO_MEASURE(7850.),#3636);
#3648=MEASURE_REPRESENTATION_ITEM('density measure',
POSITIVE_RATIO_MEASURE(7850.),#3637);
#3649=PROPERTY_DEFINITION_REPRESENTATION(#3704,#3671);
#3650=PROPERTY_DEFINITION_REPRESENTATION(#3705,#3672);
#3651=PROPERTY_DEFINITION_REPRESENTATION(#3706,#3673);
#3652=PROPERTY_DEFINITION_REPRESENTATION(#3707,#3674);
#3653=PROPERTY_DEFINITION_REPRESENTATION(#3708,#3675);
#3654=PROPERTY_DEFINITION_REPRESENTATION(#3709,#3676);
#3655=PROPERTY_DEFINITION_REPRESENTATION(#3710,#3677);
#3656=PROPERTY_DEFINITION_REPRESENTATION(#3711,#3678);
#3657=PROPERTY_DEFINITION_REPRESENTATION(#3712,#3679);
#3658=PROPERTY_DEFINITION_REPRESENTATION(#3713,#3680);
#3659=PROPERTY_DEFINITION_REPRESENTATION(#3714,#3681);
#3660=PROPERTY_DEFINITION_REPRESENTATION(#3715,#3682);
#3661=PROPERTY_DEFINITION_REPRESENTATION(#3716,#3683);
#3662=PROPERTY_DEFINITION_REPRESENTATION(#3717,#3684);
#3663=PROPERTY_DEFINITION_REPRESENTATION(#3718,#3685);
#3664=PROPERTY_DEFINITION_REPRESENTATION(#3719,#3686);
#3665=PROPERTY_DEFINITION_REPRESENTATION(#3720,#3687);
#3666=PROPERTY_DEFINITION_REPRESENTATION(#3721,#3688);
#3667=PROPERTY_DEFINITION_REPRESENTATION(#3722,#3689);
#3668=PROPERTY_DEFINITION_REPRESENTATION(#3723,#3690);
#3669=PROPERTY_DEFINITION_REPRESENTATION(#3724,#3691);
#3670=PROPERTY_DEFINITION_REPRESENTATION(#3725,#3692);
#3671=REPRESENTATION('material name',(#3693),#6085);
#3672=REPRESENTATION('density',(#3638),#6085);
#3673=REPRESENTATION('material name',(#3694),#6086);
#3674=REPRESENTATION('density',(#3639),#6086);
#3675=REPRESENTATION('material name',(#3695),#6087);
#3676=REPRESENTATION('density',(#3640),#6087);
#3677=REPRESENTATION('material name',(#3696),#6088);
#3678=REPRESENTATION('density',(#3641),#6088);
#3679=REPRESENTATION('material name',(#3697),#6089);
#3680=REPRESENTATION('density',(#3642),#6089);
#3681=REPRESENTATION('material name',(#3698),#6090);
#3682=REPRESENTATION('density',(#3643),#6090);
#3683=REPRESENTATION('material name',(#3699),#6091);
#3684=REPRESENTATION('density',(#3644),#6091);
#3685=REPRESENTATION('material name',(#3700),#6092);
#3686=REPRESENTATION('density',(#3645),#6092);
#3687=REPRESENTATION('material name',(#3701),#6093);
#3688=REPRESENTATION('density',(#3646),#6093);
#3689=REPRESENTATION('material name',(#3702),#6094);
#3690=REPRESENTATION('density',(#3647),#6094);
#3691=REPRESENTATION('material name',(#3703),#6095);
#3692=REPRESENTATION('density',(#3648),#6095);
#3693=DESCRIPTIVE_REPRESENTATION_ITEM('Steel','Steel');
#3694=DESCRIPTIVE_REPRESENTATION_ITEM('Steel','Steel');
#3695=DESCRIPTIVE_REPRESENTATION_ITEM('Steel','Steel');
#3696=DESCRIPTIVE_REPRESENTATION_ITEM('Steel','Steel');
#3697=DESCRIPTIVE_REPRESENTATION_ITEM('Steel','Steel');
#3698=DESCRIPTIVE_REPRESENTATION_ITEM('Steel','Steel');
#3699=DESCRIPTIVE_REPRESENTATION_ITEM('Steel','Steel');
#3700=DESCRIPTIVE_REPRESENTATION_ITEM('Steel','Steel');
#3701=DESCRIPTIVE_REPRESENTATION_ITEM('Steel','Steel');
#3702=DESCRIPTIVE_REPRESENTATION_ITEM('Steel','Steel');
#3703=DESCRIPTIVE_REPRESENTATION_ITEM('Steel','Steel');
#3704=PROPERTY_DEFINITION('material property','material name',#6150);
#3705=PROPERTY_DEFINITION('material property','density of part',#6150);
#3706=PROPERTY_DEFINITION('material property','material name',#6151);
#3707=PROPERTY_DEFINITION('material property','density of part',#6151);
#3708=PROPERTY_DEFINITION('material property','material name',#6152);
#3709=PROPERTY_DEFINITION('material property','density of part',#6152);
#3710=PROPERTY_DEFINITION('material property','material name',#6153);
#3711=PROPERTY_DEFINITION('material property','density of part',#6153);
#3712=PROPERTY_DEFINITION('material property','material name',#6154);
#3713=PROPERTY_DEFINITION('material property','density of part',#6154);
#3714=PROPERTY_DEFINITION('material property','material name',#6155);
#3715=PROPERTY_DEFINITION('material property','density of part',#6155);
#3716=PROPERTY_DEFINITION('material property','material name',#6156);
#3717=PROPERTY_DEFINITION('material property','density of part',#6156);
#3718=PROPERTY_DEFINITION('material property','material name',#6157);
#3719=PROPERTY_DEFINITION('material property','density of part',#6157);
#3720=PROPERTY_DEFINITION('material property','material name',#6158);
#3721=PROPERTY_DEFINITION('material property','density of part',#6158);
#3722=PROPERTY_DEFINITION('material property','material name',#6159);
#3723=PROPERTY_DEFINITION('material property','density of part',#6159);
#3724=PROPERTY_DEFINITION('material property','material name',#6160);
#3725=PROPERTY_DEFINITION('material property','density of part',#6160);
#3726=AXIS2_PLACEMENT_3D('',#5056,#4043,#4044);
#3727=AXIS2_PLACEMENT_3D('',#5057,#4045,#4046);
#3728=AXIS2_PLACEMENT_3D('',#5058,#4047,#4048);
#3729=AXIS2_PLACEMENT_3D('',#5060,#4049,#4050);
#3730=AXIS2_PLACEMENT_3D('',#5063,#4052,#4053);
#3731=AXIS2_PLACEMENT_3D('',#5064,#4054,#4055);
#3732=AXIS2_PLACEMENT_3D('',#5066,#4056,#4057);
#3733=AXIS2_PLACEMENT_3D('',#5069,#4059,#4060);
#3734=AXIS2_PLACEMENT_3D('',#5070,#4061,#4062);
#3735=AXIS2_PLACEMENT_3D('',#5079,#4067,#4068);
#3736=AXIS2_PLACEMENT_3D('',#5081,#4069,#4070);
#3737=AXIS2_PLACEMENT_3D('',#5083,#4071,#4072);
#3738=AXIS2_PLACEMENT_3D('',#5085,#4074,#4075);
#3739=AXIS2_PLACEMENT_3D('',#5091,#4079,#4080);
#3740=AXIS2_PLACEMENT_3D('',#5100,#4085,#4086);
#3741=AXIS2_PLACEMENT_3D('',#5102,#4087,#4088);
#3742=AXIS2_PLACEMENT_3D('',#5104,#4089,#4090);
#3743=AXIS2_PLACEMENT_3D('',#5106,#4092,#4093);
#3744=AXIS2_PLACEMENT_3D('',#5112,#4097,#4098);
#3745=AXIS2_PLACEMENT_3D('',#5121,#4103,#4104);
#3746=AXIS2_PLACEMENT_3D('',#5123,#4105,#4106);
#3747=AXIS2_PLACEMENT_3D('',#5125,#4107,#4108);
#3748=AXIS2_PLACEMENT_3D('',#5127,#4110,#4111);
#3749=AXIS2_PLACEMENT_3D('',#5133,#4115,#4116);
#3750=AXIS2_PLACEMENT_3D('',#5145,#4124,#4125);
#3751=AXIS2_PLACEMENT_3D('',#5149,#4128,#4129);
#3752=AXIS2_PLACEMENT_3D('',#5151,#4131,#4132);
#3753=AXIS2_PLACEMENT_3D('',#5153,#4134,#4135);
#3754=AXIS2_PLACEMENT_3D('',#5157,#4138,#4139);
#3755=AXIS2_PLACEMENT_3D('',#5166,#4144,#4145);
#3756=AXIS2_PLACEMENT_3D('',#5175,#4150,#4151);
#3757=AXIS2_PLACEMENT_3D('',#5176,#4152,#4153);
#3758=AXIS2_PLACEMENT_3D('',#5177,#4154,#4155);
#3759=AXIS2_PLACEMENT_3D('',#5178,#4156,#4157);
#3760=AXIS2_PLACEMENT_3D('',#5187,#4162,#4163);
#3761=AXIS2_PLACEMENT_3D('',#5196,#4168,#4169);
#3762=AXIS2_PLACEMENT_3D('',#5197,#4170,#4171);
#3763=AXIS2_PLACEMENT_3D('',#5198,#4172,#4173);
#3764=AXIS2_PLACEMENT_3D('',#5199,#4174,#4175);
#3765=AXIS2_PLACEMENT_3D('',#5208,#4180,#4181);
#3766=AXIS2_PLACEMENT_3D('',#5217,#4186,#4187);
#3767=AXIS2_PLACEMENT_3D('',#5218,#4188,#4189);
#3768=AXIS2_PLACEMENT_3D('',#5219,#4190,#4191);
#3769=AXIS2_PLACEMENT_3D('',#5220,#4192,#4193);
#3770=AXIS2_PLACEMENT_3D('',#5226,#4197,#4198);
#3771=AXIS2_PLACEMENT_3D('',#5229,#4201,#4202);
#3772=AXIS2_PLACEMENT_3D('',#5235,#4206,#4207);
#3773=AXIS2_PLACEMENT_3D('',#5238,#4210,#4211);
#3774=AXIS2_PLACEMENT_3D('',#5241,#4214,#4215);
#3775=AXIS2_PLACEMENT_3D('',#5250,#4220,#4221);
#3776=AXIS2_PLACEMENT_3D('',#5256,#4225,#4226);
#3777=AXIS2_PLACEMENT_3D('',#5260,#4229,#4230);
#3778=AXIS2_PLACEMENT_3D('',#5264,#4233,#4234);
#3779=AXIS2_PLACEMENT_3D('',#5266,#4236,#4237);
#3780=AXIS2_PLACEMENT_3D('',#5282,#4246,#4247);
#3781=AXIS2_PLACEMENT_3D('',#5286,#4250,#4251);
#3782=AXIS2_PLACEMENT_3D('',#5290,#4254,#4255);
#3783=AXIS2_PLACEMENT_3D('',#5294,#4258,#4259);
#3784=AXIS2_PLACEMENT_3D('',#5298,#4262,#4263);
#3785=AXIS2_PLACEMENT_3D('',#5302,#4266,#4267);
#3786=AXIS2_PLACEMENT_3D('',#5306,#4270,#4271);
#3787=AXIS2_PLACEMENT_3D('',#5310,#4274,#4275);
#3788=AXIS2_PLACEMENT_3D('',#5312,#4277,#4278);
#3789=AXIS2_PLACEMENT_3D('',#5313,#4279,#4280);
#3790=AXIS2_PLACEMENT_3D('',#5314,#4281,#4282);
#3791=AXIS2_PLACEMENT_3D('',#5316,#4283,#4284);
#3792=AXIS2_PLACEMENT_3D('',#5318,#4285,#4286);
#3793=AXIS2_PLACEMENT_3D('',#5320,#4287,#4288);
#3794=AXIS2_PLACEMENT_3D('',#5321,#4289,#4290);
#3795=AXIS2_PLACEMENT_3D('',#5322,#4291,#4292);
#3796=AXIS2_PLACEMENT_3D('',#5326,#4294,#4295);
#3797=AXIS2_PLACEMENT_3D('',#5327,#4296,#4297);
#3798=AXIS2_PLACEMENT_3D('',#5328,#4298,#4299);
#3799=AXIS2_PLACEMENT_3D('',#5330,#4300,#4301);
#3800=AXIS2_PLACEMENT_3D('',#5331,#4302,#4303);
#3801=AXIS2_PLACEMENT_3D('',#5333,#4304,#4305);
#3802=AXIS2_PLACEMENT_3D('',#5334,#4306,#4307);
#3803=AXIS2_PLACEMENT_3D('',#5335,#4308,#4309);
#3804=AXIS2_PLACEMENT_3D('',#5337,#4310,#4311);
#3805=AXIS2_PLACEMENT_3D('',#5338,#4312,#4313);
#3806=AXIS2_PLACEMENT_3D('',#5340,#4315,#4316);
#3807=AXIS2_PLACEMENT_3D('',#5341,#4317,#4318);
#3808=AXIS2_PLACEMENT_3D('',#5343,#4319,#4320);
#3809=AXIS2_PLACEMENT_3D('',#5346,#4322,#4323);
#3810=AXIS2_PLACEMENT_3D('',#5347,#4324,#4325);
#3811=AXIS2_PLACEMENT_3D('',#5356,#4330,#4331);
#3812=AXIS2_PLACEMENT_3D('',#5365,#4336,#4337);
#3813=AXIS2_PLACEMENT_3D('',#5368,#4340,#4341);
#3814=AXIS2_PLACEMENT_3D('',#5374,#4345,#4346);
#3815=AXIS2_PLACEMENT_3D('',#5380,#4350,#4351);
#3816=AXIS2_PLACEMENT_3D('',#5383,#4352,#4353);
#3817=AXIS2_PLACEMENT_3D('',#5385,#4355,#4356);
#3818=AXIS2_PLACEMENT_3D('',#5388,#4357,#4358);
#3819=AXIS2_PLACEMENT_3D('',#5390,#4359,#4360);
#3820=AXIS2_PLACEMENT_3D('',#5392,#4362,#4363);
#3821=AXIS2_PLACEMENT_3D('',#5395,#4364,#4365);
#3822=AXIS2_PLACEMENT_3D('',#5397,#4366,#4367);
#3823=AXIS2_PLACEMENT_3D('',#5399,#4369,#4370);
#3824=AXIS2_PLACEMENT_3D('',#5402,#4371,#4372);
#3825=AXIS2_PLACEMENT_3D('',#5404,#4374,#4375);
#3826=AXIS2_PLACEMENT_3D('',#5412,#4381,#4382);
#3827=AXIS2_PLACEMENT_3D('',#5420,#4388,#4389);
#3828=AXIS2_PLACEMENT_3D('',#5421,#4390,#4391);
#3829=AXIS2_PLACEMENT_3D('',#5422,#4392,#4393);
#3830=AXIS2_PLACEMENT_3D('',#5428,#4397,#4398);
#3831=AXIS2_PLACEMENT_3D('',#5435,#4402,#4403);
#3832=AXIS2_PLACEMENT_3D('',#5436,#4404,#4405);
#3833=AXIS2_PLACEMENT_3D('',#5438,#4406,#4407);
#3834=AXIS2_PLACEMENT_3D('',#5439,#4408,#4409);
#3835=AXIS2_PLACEMENT_3D('',#5440,#4410,#4411);
#3836=AXIS2_PLACEMENT_3D('',#5442,#4412,#4413);
#3837=AXIS2_PLACEMENT_3D('',#5444,#4415,#4416);
#3838=AXIS2_PLACEMENT_3D('',#5446,#4417,#4418);
#3839=AXIS2_PLACEMENT_3D('',#5448,#4420,#4421);
#3840=AXIS2_PLACEMENT_3D('',#5450,#4422,#4423);
#3841=AXIS2_PLACEMENT_3D('',#5452,#4425,#4426);
#3842=AXIS2_PLACEMENT_3D('',#5454,#4427,#4428);
#3843=AXIS2_PLACEMENT_3D('',#5456,#4430,#4431);
#3844=AXIS2_PLACEMENT_3D('',#5462,#4435,#4436);
#3845=AXIS2_PLACEMENT_3D('',#5468,#4440,#4441);
#3846=AXIS2_PLACEMENT_3D('',#5474,#4445,#4446);
#3847=AXIS2_PLACEMENT_3D('',#5483,#4451,#4452);
#3848=AXIS2_PLACEMENT_3D('',#5486,#4455,#4456);
#3849=AXIS2_PLACEMENT_3D('',#5498,#4463,#4464);
#3850=AXIS2_PLACEMENT_3D('',#5502,#4467,#4468);
#3851=AXIS2_PLACEMENT_3D('',#5506,#4471,#4472);
#3852=AXIS2_PLACEMENT_3D('',#5510,#4475,#4476);
#3853=AXIS2_PLACEMENT_3D('',#5514,#4479,#4480);
#3854=AXIS2_PLACEMENT_3D('',#5518,#4483,#4484);
#3855=AXIS2_PLACEMENT_3D('',#5520,#4486,#4487);
#3856=AXIS2_PLACEMENT_3D('',#5521,#4488,#4489);
#3857=AXIS2_PLACEMENT_3D('',#5522,#4490,#4491);
#3858=AXIS2_PLACEMENT_3D('',#5525,#4492,#4493);
#3859=AXIS2_PLACEMENT_3D('',#5529,#4495,#4496);
#3860=AXIS2_PLACEMENT_3D('',#5531,#4498,#4499);
#3861=AXIS2_PLACEMENT_3D('',#5535,#4501,#4502);
#3862=AXIS2_PLACEMENT_3D('',#5539,#4504,#4505);
#3863=AXIS2_PLACEMENT_3D('',#5543,#4507,#4508);
#3864=AXIS2_PLACEMENT_3D('',#5545,#4510,#4511);
#3865=AXIS2_PLACEMENT_3D('',#5549,#4514,#4515);
#3866=AXIS2_PLACEMENT_3D('',#5551,#4516,#4517);
#3867=AXIS2_PLACEMENT_3D('',#5553,#4519,#4520);
#3868=AXIS2_PLACEMENT_3D('',#5556,#4521,#4522);
#3869=AXIS2_PLACEMENT_3D('',#5559,#4525,#4526);
#3870=AXIS2_PLACEMENT_3D('',#5563,#4529,#4530);
#3871=AXIS2_PLACEMENT_3D('',#5565,#4531,#4532);
#3872=AXIS2_PLACEMENT_3D('',#5567,#4534,#4535);
#3873=AXIS2_PLACEMENT_3D('',#5569,#4537,#4538);
#3874=AXIS2_PLACEMENT_3D('',#5571,#4540,#4541);
#3875=AXIS2_PLACEMENT_3D('',#5572,#4542,#4543);
#3876=AXIS2_PLACEMENT_3D('',#5573,#4544,#4545);
#3877=AXIS2_PLACEMENT_3D('',#5575,#4546,#4547);
#3878=AXIS2_PLACEMENT_3D('',#5578,#4549,#4550);
#3879=AXIS2_PLACEMENT_3D('',#5579,#4551,#4552);
#3880=AXIS2_PLACEMENT_3D('',#5580,#4553,#4554);
#3881=AXIS2_PLACEMENT_3D('',#5582,#4555,#4556);
#3882=AXIS2_PLACEMENT_3D('',#5585,#4558,#4559);
#3883=AXIS2_PLACEMENT_3D('',#5586,#4560,#4561);
#3884=AXIS2_PLACEMENT_3D('',#5587,#4562,#4563);
#3885=AXIS2_PLACEMENT_3D('',#5588,#4564,#4565);
#3886=AXIS2_PLACEMENT_3D('',#5589,#4566,#4567);
#3887=AXIS2_PLACEMENT_3D('',#5591,#4568,#4569);
#3888=AXIS2_PLACEMENT_3D('',#5594,#4571,#4572);
#3889=AXIS2_PLACEMENT_3D('',#5595,#4573,#4574);
#3890=AXIS2_PLACEMENT_3D('',#5604,#4579,#4580);
#3891=AXIS2_PLACEMENT_3D('',#5610,#4584,#4585);
#3892=AXIS2_PLACEMENT_3D('',#5616,#4589,#4590);
#3893=AXIS2_PLACEMENT_3D('',#5619,#4593,#4594);
#3894=AXIS2_PLACEMENT_3D('',#5628,#4599,#4600);
#3895=AXIS2_PLACEMENT_3D('',#5634,#4604,#4605);
#3896=AXIS2_PLACEMENT_3D('',#5646,#4612,#4613);
#3897=AXIS2_PLACEMENT_3D('',#5652,#4617,#4618);
#3898=AXIS2_PLACEMENT_3D('',#5656,#4621,#4622);
#3899=AXIS2_PLACEMENT_3D('',#5660,#4625,#4626);
#3900=AXIS2_PLACEMENT_3D('',#5664,#4629,#4630);
#3901=AXIS2_PLACEMENT_3D('',#5666,#4632,#4633);
#3902=AXIS2_PLACEMENT_3D('',#5668,#4635,#4636);
#3903=AXIS2_PLACEMENT_3D('',#5669,#4637,#4638);
#3904=AXIS2_PLACEMENT_3D('',#5670,#4639,#4640);
#3905=AXIS2_PLACEMENT_3D('',#5672,#4641,#4642);
#3906=AXIS2_PLACEMENT_3D('',#5674,#4643,#4644);
#3907=AXIS2_PLACEMENT_3D('',#5675,#4645,#4646);
#3908=AXIS2_PLACEMENT_3D('',#5676,#4647,#4648);
#3909=AXIS2_PLACEMENT_3D('',#5678,#4649,#4650);
#3910=AXIS2_PLACEMENT_3D('',#5680,#4652,#4653);
#3911=AXIS2_PLACEMENT_3D('',#5682,#4654,#4655);
#3912=AXIS2_PLACEMENT_3D('',#5683,#4656,#4657);
#3913=AXIS2_PLACEMENT_3D('',#5685,#4658,#4659);
#3914=AXIS2_PLACEMENT_3D('',#5687,#4660,#4661);
#3915=AXIS2_PLACEMENT_3D('',#5688,#4662,#4663);
#3916=AXIS2_PLACEMENT_3D('',#5689,#4664,#4665);
#3917=AXIS2_PLACEMENT_3D('',#5691,#4666,#4667);
#3918=AXIS2_PLACEMENT_3D('',#5693,#4669,#4670);
#3919=AXIS2_PLACEMENT_3D('',#5695,#4671,#4672);
#3920=AXIS2_PLACEMENT_3D('',#5696,#4673,#4674);
#3921=AXIS2_PLACEMENT_3D('',#5698,#4675,#4676);
#3922=AXIS2_PLACEMENT_3D('',#5699,#4677,#4678);
#3923=AXIS2_PLACEMENT_3D('',#5700,#4679,#4680);
#3924=AXIS2_PLACEMENT_3D('',#5701,#4681,#4682);
#3925=AXIS2_PLACEMENT_3D('',#5702,#4683,#4684);
#3926=AXIS2_PLACEMENT_3D('',#5703,#4685,#4686);
#3927=AXIS2_PLACEMENT_3D('',#5705,#4687,#4688);
#3928=AXIS2_PLACEMENT_3D('',#5706,#4689,#4690);
#3929=AXIS2_PLACEMENT_3D('',#5707,#4691,#4692);
#3930=AXIS2_PLACEMENT_3D('',#5710,#4694,#4695);
#3931=AXIS2_PLACEMENT_3D('',#5711,#4696,#4697);
#3932=AXIS2_PLACEMENT_3D('',#5712,#4698,#4699);
#3933=AXIS2_PLACEMENT_3D('',#5713,#4700,#4701);
#3934=AXIS2_PLACEMENT_3D('',#5715,#4702,#4703);
#3935=AXIS2_PLACEMENT_3D('',#5718,#4705,#4706);
#3936=AXIS2_PLACEMENT_3D('',#5719,#4707,#4708);
#3937=AXIS2_PLACEMENT_3D('',#5721,#4709,#4710);
#3938=AXIS2_PLACEMENT_3D('',#5724,#4712,#4713);
#3939=AXIS2_PLACEMENT_3D('',#5725,#4714,#4715);
#3940=AXIS2_PLACEMENT_3D('',#5727,#4716,#4717);
#3941=AXIS2_PLACEMENT_3D('',#5730,#4719,#4720);
#3942=AXIS2_PLACEMENT_3D('',#5731,#4721,#4722);
#3943=AXIS2_PLACEMENT_3D('',#5733,#4723,#4724);
#3944=AXIS2_PLACEMENT_3D('',#5736,#4726,#4727);
#3945=AXIS2_PLACEMENT_3D('',#5737,#4728,#4729);
#3946=AXIS2_PLACEMENT_3D('',#5746,#4734,#4735);
#3947=AXIS2_PLACEMENT_3D('',#5752,#4739,#4740);
#3948=AXIS2_PLACEMENT_3D('',#5758,#4744,#4745);
#3949=AXIS2_PLACEMENT_3D('',#5764,#4749,#4750);
#3950=AXIS2_PLACEMENT_3D('',#5770,#4754,#4755);
#3951=AXIS2_PLACEMENT_3D('',#5776,#4759,#4760);
#3952=AXIS2_PLACEMENT_3D('',#5782,#4764,#4765);
#3953=AXIS2_PLACEMENT_3D('',#5788,#4769,#4770);
#3954=AXIS2_PLACEMENT_3D('',#5794,#4774,#4775);
#3955=AXIS2_PLACEMENT_3D('',#5797,#4778,#4779);
#3956=AXIS2_PLACEMENT_3D('',#5798,#4780,#4781);
#3957=AXIS2_PLACEMENT_3D('',#5799,#4782,#4783);
#3958=AXIS2_PLACEMENT_3D('',#5800,#4784,#4785);
#3959=AXIS2_PLACEMENT_3D('',#5802,#4786,#4787);
#3960=AXIS2_PLACEMENT_3D('',#5805,#4789,#4790);
#3961=AXIS2_PLACEMENT_3D('',#5806,#4791,#4792);
#3962=AXIS2_PLACEMENT_3D('',#5808,#4793,#4794);
#3963=AXIS2_PLACEMENT_3D('',#5811,#4796,#4797);
#3964=AXIS2_PLACEMENT_3D('',#5812,#4798,#4799);
#3965=AXIS2_PLACEMENT_3D('',#5814,#4800,#4801);
#3966=AXIS2_PLACEMENT_3D('',#5817,#4803,#4804);
#3967=AXIS2_PLACEMENT_3D('',#5818,#4805,#4806);
#3968=AXIS2_PLACEMENT_3D('',#5820,#4807,#4808);
#3969=AXIS2_PLACEMENT_3D('',#5823,#4810,#4811);
#3970=AXIS2_PLACEMENT_3D('',#5824,#4812,#4813);
#3971=AXIS2_PLACEMENT_3D('',#5833,#4818,#4819);
#3972=AXIS2_PLACEMENT_3D('',#5839,#4823,#4824);
#3973=AXIS2_PLACEMENT_3D('',#5845,#4828,#4829);
#3974=AXIS2_PLACEMENT_3D('',#5851,#4833,#4834);
#3975=AXIS2_PLACEMENT_3D('',#5857,#4838,#4839);
#3976=AXIS2_PLACEMENT_3D('',#5863,#4843,#4844);
#3977=AXIS2_PLACEMENT_3D('',#5869,#4848,#4849);
#3978=AXIS2_PLACEMENT_3D('',#5875,#4853,#4854);
#3979=AXIS2_PLACEMENT_3D('',#5881,#4858,#4859);
#3980=AXIS2_PLACEMENT_3D('',#5884,#4862,#4863);
#3981=AXIS2_PLACEMENT_3D('',#5885,#4864,#4865);
#3982=AXIS2_PLACEMENT_3D('',#5886,#4866,#4867);
#3983=AXIS2_PLACEMENT_3D('',#5887,#4868,#4869);
#3984=AXIS2_PLACEMENT_3D('',#5889,#4870,#4871);
#3985=AXIS2_PLACEMENT_3D('',#5892,#4873,#4874);
#3986=AXIS2_PLACEMENT_3D('',#5893,#4875,#4876);
#3987=AXIS2_PLACEMENT_3D('',#5895,#4877,#4878);
#3988=AXIS2_PLACEMENT_3D('',#5898,#4880,#4881);
#3989=AXIS2_PLACEMENT_3D('',#5899,#4882,#4883);
#3990=AXIS2_PLACEMENT_3D('',#5901,#4884,#4885);
#3991=AXIS2_PLACEMENT_3D('',#5904,#4887,#4888);
#3992=AXIS2_PLACEMENT_3D('',#5905,#4889,#4890);
#3993=AXIS2_PLACEMENT_3D('',#5907,#4891,#4892);
#3994=AXIS2_PLACEMENT_3D('',#5910,#4894,#4895);
#3995=AXIS2_PLACEMENT_3D('',#5911,#4896,#4897);
#3996=AXIS2_PLACEMENT_3D('',#5920,#4902,#4903);
#3997=AXIS2_PLACEMENT_3D('',#5926,#4907,#4908);
#3998=AXIS2_PLACEMENT_3D('',#5932,#4912,#4913);
#3999=AXIS2_PLACEMENT_3D('',#5938,#4917,#4918);
#4000=AXIS2_PLACEMENT_3D('',#5944,#4922,#4923);
#4001=AXIS2_PLACEMENT_3D('',#5950,#4927,#4928);
#4002=AXIS2_PLACEMENT_3D('',#5956,#4932,#4933);
#4003=AXIS2_PLACEMENT_3D('',#5962,#4937,#4938);
#4004=AXIS2_PLACEMENT_3D('',#5968,#4942,#4943);
#4005=AXIS2_PLACEMENT_3D('',#5971,#4946,#4947);
#4006=AXIS2_PLACEMENT_3D('',#5972,#4948,#4949);
#4007=AXIS2_PLACEMENT_3D('',#5973,#4950,#4951);
#4008=AXIS2_PLACEMENT_3D('',#5974,#4952,#4953);
#4009=AXIS2_PLACEMENT_3D('',#5976,#4954,#4955);
#4010=AXIS2_PLACEMENT_3D('',#5979,#4957,#4958);
#4011=AXIS2_PLACEMENT_3D('',#5980,#4959,#4960);
#4012=AXIS2_PLACEMENT_3D('',#5982,#4961,#4962);
#4013=AXIS2_PLACEMENT_3D('',#5985,#4964,#4965);
#4014=AXIS2_PLACEMENT_3D('',#5986,#4966,#4967);
#4015=AXIS2_PLACEMENT_3D('',#5988,#4968,#4969);
#4016=AXIS2_PLACEMENT_3D('',#5991,#4971,#4972);
#4017=AXIS2_PLACEMENT_3D('',#5992,#4973,#4974);
#4018=AXIS2_PLACEMENT_3D('',#5994,#4975,#4976);
#4019=AXIS2_PLACEMENT_3D('',#5997,#4978,#4979);
#4020=AXIS2_PLACEMENT_3D('',#5998,#4980,#4981);
#4021=AXIS2_PLACEMENT_3D('',#6007,#4986,#4987);
#4022=AXIS2_PLACEMENT_3D('',#6013,#4991,#4992);
#4023=AXIS2_PLACEMENT_3D('',#6019,#4996,#4997);
#4024=AXIS2_PLACEMENT_3D('',#6025,#5001,#5002);
#4025=AXIS2_PLACEMENT_3D('',#6031,#5006,#5007);
#4026=AXIS2_PLACEMENT_3D('',#6037,#5011,#5012);
#4027=AXIS2_PLACEMENT_3D('',#6043,#5016,#5017);
#4028=AXIS2_PLACEMENT_3D('',#6049,#5021,#5022);
#4029=AXIS2_PLACEMENT_3D('',#6055,#5026,#5027);
#4030=AXIS2_PLACEMENT_3D('',#6058,#5030,#5031);
#4031=AXIS2_PLACEMENT_3D('',#6059,#5032,#5033);
#4032=AXIS2_PLACEMENT_3D('',#6060,#5034,#5035);
#4033=AXIS2_PLACEMENT_3D('',#6061,#5036,#5037);
#4034=AXIS2_PLACEMENT_3D('',#6062,#5038,#5039);
#4035=AXIS2_PLACEMENT_3D('',#6063,#5040,#5041);
#4036=AXIS2_PLACEMENT_3D('',#6064,#5042,#5043);
#4037=AXIS2_PLACEMENT_3D('',#6065,#5044,#5045);
#4038=AXIS2_PLACEMENT_3D('',#6066,#5046,#5047);
#4039=AXIS2_PLACEMENT_3D('',#6067,#5048,#5049);
#4040=AXIS2_PLACEMENT_3D('',#6068,#5050,#5051);
#4041=AXIS2_PLACEMENT_3D('',#6069,#5052,#5053);
#4042=AXIS2_PLACEMENT_3D('',#6070,#5054,#5055);
#4043=DIRECTION('axis',(0.,0.,1.));
#4044=DIRECTION('refdir',(1.,0.,0.));
#4045=DIRECTION('axis',(0.,0.,1.));
#4046=DIRECTION('refdir',(1.,0.,0.));
#4047=DIRECTION('center_axis',(0.,-1.,0.));
#4048=DIRECTION('ref_axis',(-1.,0.,0.));
#4049=DIRECTION('center_axis',(0.,-1.,0.));
#4050=DIRECTION('ref_axis',(-1.,0.,0.));
#4051=DIRECTION('',(0.,-1.,0.));
#4052=DIRECTION('center_axis',(0.,1.,0.));
#4053=DIRECTION('ref_axis',(-1.,0.,0.));
#4054=DIRECTION('center_axis',(0.,-1.,0.));
#4055=DIRECTION('ref_axis',(-1.,0.,0.));
#4056=DIRECTION('center_axis',(0.,-1.,0.));
#4057=DIRECTION('ref_axis',(-1.,0.,0.));
#4058=DIRECTION('',(0.,-1.,0.));
#4059=DIRECTION('center_axis',(0.,1.,0.));
#4060=DIRECTION('ref_axis',(-1.,0.,0.));
#4061=DIRECTION('center_axis',(0.,-1.,0.));
#4062=DIRECTION('ref_axis',(1.,0.,0.));
#4063=DIRECTION('',(0.,0.,1.));
#4064=DIRECTION('',(-1.,0.,0.));
#4065=DIRECTION('',(0.,0.,1.));
#4066=DIRECTION('',(1.,0.,0.));
#4067=DIRECTION('center_axis',(0.,0.,-1.));
#4068=DIRECTION('ref_axis',(0.,1.,0.));
#4069=DIRECTION('center_axis',(0.,0.,-1.));
#4070=DIRECTION('ref_axis',(0.,1.,0.));
#4071=DIRECTION('center_axis',(0.,0.,1.));
#4072=DIRECTION('ref_axis',(0.,1.,0.));
#4073=DIRECTION('',(0.,0.,1.));
#4074=DIRECTION('center_axis',(-1.98507404446773E-15,1.,0.));
#4075=DIRECTION('ref_axis',(-1.,-1.98507404446773E-15,0.));
#4076=DIRECTION('',(0.,0.,-1.));
#4077=DIRECTION('',(-1.,-1.98507404446773E-15,0.));
#4078=DIRECTION('',(1.,1.98507404446773E-15,0.));
#4079=DIRECTION('center_axis',(-4.96268511116933E-16,-1.,0.));
#4080=DIRECTION('ref_axis',(1.,-4.96268511116933E-16,0.));
#4081=DIRECTION('',(0.,0.,1.));
#4082=DIRECTION('',(-1.,4.96268511116933E-16,0.));
#4083=DIRECTION('',(0.,0.,1.));
#4084=DIRECTION('',(1.,-4.96268511116933E-16,0.));
#4085=DIRECTION('center_axis',(0.,0.,-1.));
#4086=DIRECTION('ref_axis',(0.,1.,0.));
#4087=DIRECTION('center_axis',(0.,0.,-1.));
#4088=DIRECTION('ref_axis',(0.,1.,0.));
#4089=DIRECTION('center_axis',(0.,0.,1.));
#4090=DIRECTION('ref_axis',(0.,1.,0.));
#4091=DIRECTION('',(0.,0.,1.));
#4092=DIRECTION('center_axis',(-1.4888055333508E-15,1.,0.));
#4093=DIRECTION('ref_axis',(-1.,-1.4888055333508E-15,0.));
#4094=DIRECTION('',(0.,0.,-1.));
#4095=DIRECTION('',(-1.,-1.4888055333508E-15,0.));
#4096=DIRECTION('',(1.,1.4888055333508E-15,0.));
#4097=DIRECTION('center_axis',(-9.92537022233866E-16,-1.,0.));
#4098=DIRECTION('ref_axis',(1.,-9.92537022233866E-16,0.));
#4099=DIRECTION('',(0.,0.,1.));
#4100=DIRECTION('',(-1.,9.92537022233866E-16,0.));
#4101=DIRECTION('',(0.,0.,1.));
#4102=DIRECTION('',(1.,-9.92537022233866E-16,0.));
#4103=DIRECTION('center_axis',(0.,0.,-1.));
#4104=DIRECTION('ref_axis',(0.,1.,0.));
#4105=DIRECTION('center_axis',(0.,0.,-1.));
#4106=DIRECTION('ref_axis',(0.,1.,0.));
#4107=DIRECTION('center_axis',(0.,0.,1.));
#4108=DIRECTION('ref_axis',(0.,1.,0.));
#4109=DIRECTION('',(0.,0.,1.));
#4110=DIRECTION('center_axis',(-1.98507404446773E-15,1.,0.));
#4111=DIRECTION('ref_axis',(-1.,-1.98507404446773E-15,0.));
#4112=DIRECTION('',(0.,0.,-1.));
#4113=DIRECTION('',(-1.,-1.98507404446773E-15,0.));
#4114=DIRECTION('',(1.,1.98507404446773E-15,0.));
#4115=DIRECTION('center_axis',(0.,0.,1.));
#4116=DIRECTION('ref_axis',(1.,0.,0.));
#4117=DIRECTION('',(0.,1.,0.));
#4118=DIRECTION('',(0.,1.,0.));
#4119=DIRECTION('',(0.,1.,0.));
#4120=DIRECTION('',(1.,0.,0.));
#4121=DIRECTION('',(0.,1.,0.));
#4122=DIRECTION('',(1.,0.,0.));
#4123=DIRECTION('',(0.,1.,0.));
#4124=DIRECTION('center_axis',(-1.,0.,0.));
#4125=DIRECTION('ref_axis',(0.,0.,1.));
#4126=DIRECTION('',(0.,1.,0.));
#4127=DIRECTION('',(0.,0.,1.));
#4128=DIRECTION('center_axis',(-1.,0.,0.));
#4129=DIRECTION('ref_axis',(0.,0.,1.));
#4130=DIRECTION('',(0.,1.,0.));
#4131=DIRECTION('center_axis',(-1.,0.,0.));
#4132=DIRECTION('ref_axis',(0.,0.,1.));
#4133=DIRECTION('',(0.,1.,0.));
#4134=DIRECTION('center_axis',(-1.,0.,0.));
#4135=DIRECTION('ref_axis',(0.,0.,1.));
#4136=DIRECTION('',(0.,0.,1.));
#4137=DIRECTION('',(0.,1.,0.));
#4138=DIRECTION('center_axis',(-4.96268511116933E-16,1.,0.));
#4139=DIRECTION('ref_axis',(-1.,-4.96268511116933E-16,0.));
#4140=DIRECTION('',(1.,4.96268511116933E-16,0.));
#4141=DIRECTION('',(0.,0.,1.));
#4142=DIRECTION('',(-1.,-4.96268511116933E-16,0.));
#4143=DIRECTION('',(0.,0.,-1.));
#4144=DIRECTION('center_axis',(-1.4888055333508E-15,-1.,0.));
#4145=DIRECTION('ref_axis',(1.,-1.4888055333508E-15,0.));
#4146=DIRECTION('',(-1.,1.4888055333508E-15,0.));
#4147=DIRECTION('',(0.,0.,1.));
#4148=DIRECTION('',(1.,-1.4888055333508E-15,0.));
#4149=DIRECTION('',(0.,0.,1.));
#4150=DIRECTION('center_axis',(0.,0.,1.));
#4151=DIRECTION('ref_axis',(0.,1.,0.));
#4152=DIRECTION('center_axis',(0.,0.,-1.));
#4153=DIRECTION('ref_axis',(0.,1.,0.));
#4154=DIRECTION('center_axis',(0.,0.,1.));
#4155=DIRECTION('ref_axis',(0.,1.,0.));
#4156=DIRECTION('center_axis',(-9.92537022233866E-16,1.,0.));
#4157=DIRECTION('ref_axis',(-1.,-9.92537022233866E-16,0.));
#4158=DIRECTION('',(1.,9.92537022233866E-16,0.));
#4159=DIRECTION('',(0.,0.,1.));
#4160=DIRECTION('',(-1.,-9.92537022233866E-16,0.));
#4161=DIRECTION('',(0.,0.,-1.));
#4162=DIRECTION('center_axis',(-1.98507404446773E-15,-1.,0.));
#4163=DIRECTION('ref_axis',(1.,-1.98507404446773E-15,0.));
#4164=DIRECTION('',(-1.,1.98507404446773E-15,0.));
#4165=DIRECTION('',(0.,0.,1.));
#4166=DIRECTION('',(1.,-1.98507404446773E-15,0.));
#4167=DIRECTION('',(0.,0.,1.));
#4168=DIRECTION('center_axis',(0.,0.,1.));
#4169=DIRECTION('ref_axis',(0.,1.,0.));
#4170=DIRECTION('center_axis',(0.,0.,-1.));
#4171=DIRECTION('ref_axis',(0.,1.,0.));
#4172=DIRECTION('center_axis',(0.,0.,1.));
#4173=DIRECTION('ref_axis',(0.,1.,0.));
#4174=DIRECTION('center_axis',(0.,1.,0.));
#4175=DIRECTION('ref_axis',(-1.,0.,0.));
#4176=DIRECTION('',(1.,0.,0.));
#4177=DIRECTION('',(0.,0.,1.));
#4178=DIRECTION('',(-1.,0.,0.));
#4179=DIRECTION('',(0.,0.,-1.));
#4180=DIRECTION('center_axis',(-1.98507404446773E-15,-1.,0.));
#4181=DIRECTION('ref_axis',(1.,-1.98507404446773E-15,0.));
#4182=DIRECTION('',(-1.,1.98507404446773E-15,0.));
#4183=DIRECTION('',(0.,0.,1.));
#4184=DIRECTION('',(1.,-1.98507404446773E-15,0.));
#4185=DIRECTION('',(0.,0.,1.));
#4186=DIRECTION('center_axis',(0.,0.,1.));
#4187=DIRECTION('ref_axis',(0.,1.,0.));
#4188=DIRECTION('center_axis',(0.,0.,-1.));
#4189=DIRECTION('ref_axis',(0.,1.,0.));
#4190=DIRECTION('center_axis',(0.,0.,1.));
#4191=DIRECTION('ref_axis',(0.,1.,0.));
#4192=DIRECTION('center_axis',(1.,0.,0.));
#4193=DIRECTION('ref_axis',(0.,0.,-1.));
#4194=DIRECTION('',(0.,1.,0.));
#4195=DIRECTION('',(0.,0.,-1.));
#4196=DIRECTION('',(0.,1.,0.));
#4197=DIRECTION('center_axis',(1.,0.,0.));
#4198=DIRECTION('ref_axis',(0.,0.,-1.));
#4199=DIRECTION('',(0.,1.,0.));
#4200=DIRECTION('',(0.,1.,0.));
#4201=DIRECTION('center_axis',(1.,0.,0.));
#4202=DIRECTION('ref_axis',(0.,0.,-1.));
#4203=DIRECTION('',(0.,1.,0.));
#4204=DIRECTION('',(0.,0.,-1.));
#4205=DIRECTION('',(0.,1.,0.));
#4206=DIRECTION('center_axis',(1.,0.,0.));
#4207=DIRECTION('ref_axis',(0.,0.,-1.));
#4208=DIRECTION('',(0.,1.,0.));
#4209=DIRECTION('',(0.,1.,0.));
#4210=DIRECTION('center_axis',(0.,0.,-1.));
#4211=DIRECTION('ref_axis',(-1.,0.,0.));
#4212=DIRECTION('',(-1.,0.,0.));
#4213=DIRECTION('',(-1.,0.,0.));
#4214=DIRECTION('center_axis',(0.,1.,0.));
#4215=DIRECTION('ref_axis',(0.,0.,1.));
#4216=DIRECTION('',(1.,0.,0.));
#4217=DIRECTION('',(0.,0.,1.));
#4218=DIRECTION('',(-1.,0.,0.));
#4219=DIRECTION('',(0.,0.,-1.));
#4220=DIRECTION('center_axis',(-1.,0.,0.));
#4221=DIRECTION('ref_axis',(0.,0.,1.));
#4222=DIRECTION('',(0.,1.,0.));
#4223=DIRECTION('',(0.,0.,1.));
#4224=DIRECTION('',(0.,1.,0.));
#4225=DIRECTION('center_axis',(0.,0.,1.));
#4226=DIRECTION('ref_axis',(1.,0.,0.));
#4227=DIRECTION('',(0.,1.,0.));
#4228=DIRECTION('',(1.,0.,0.));
#4229=DIRECTION('center_axis',(1.,0.,0.));
#4230=DIRECTION('ref_axis',(0.,0.,-1.));
#4231=DIRECTION('',(0.,1.,0.));
#4232=DIRECTION('',(0.,0.,-1.));
#4233=DIRECTION('center_axis',(0.,1.,0.));
#4234=DIRECTION('ref_axis',(0.,0.,1.));
#4235=DIRECTION('',(1.,0.,0.));
#4236=DIRECTION('center_axis',(0.,1.,0.));
#4237=DIRECTION('ref_axis',(0.,0.,1.));
#4238=DIRECTION('',(1.,0.,0.));
#4239=DIRECTION('',(0.,0.,1.));
#4240=DIRECTION('',(-1.,0.,0.));
#4241=DIRECTION('',(0.,0.,1.));
#4242=DIRECTION('',(1.,0.,0.));
#4243=DIRECTION('',(0.,0.,-1.));
#4244=DIRECTION('',(-1.,0.,0.));
#4245=DIRECTION('',(0.,0.,-1.));
#4246=DIRECTION('center_axis',(-1.,0.,0.));
#4247=DIRECTION('ref_axis',(0.,0.,1.));
#4248=DIRECTION('',(0.,1.,0.));
#4249=DIRECTION('',(0.,0.,1.));
#4250=DIRECTION('center_axis',(0.,0.,-1.));
#4251=DIRECTION('ref_axis',(-1.,0.,0.));
#4252=DIRECTION('',(0.,1.,0.));
#4253=DIRECTION('',(-1.,0.,0.));
#4254=DIRECTION('center_axis',(-1.,0.,0.));
#4255=DIRECTION('ref_axis',(0.,0.,1.));
#4256=DIRECTION('',(0.,1.,0.));
#4257=DIRECTION('',(0.,0.,1.));
#4258=DIRECTION('center_axis',(0.,0.,1.));
#4259=DIRECTION('ref_axis',(1.,0.,0.));
#4260=DIRECTION('',(1.,0.,0.));
#4261=DIRECTION('',(0.,1.,0.));
#4262=DIRECTION('center_axis',(0.,0.,1.));
#4263=DIRECTION('ref_axis',(1.,0.,0.));
#4264=DIRECTION('',(1.,0.,0.));
#4265=DIRECTION('',(0.,1.,0.));
#4266=DIRECTION('center_axis',(1.,0.,0.));
#4267=DIRECTION('ref_axis',(0.,0.,-1.));
#4268=DIRECTION('',(0.,0.,-1.));
#4269=DIRECTION('',(0.,1.,0.));
#4270=DIRECTION('center_axis',(0.,0.,-1.));
#4271=DIRECTION('ref_axis',(-1.,0.,0.));
#4272=DIRECTION('',(-1.,0.,0.));
#4273=DIRECTION('',(0.,1.,0.));
#4274=DIRECTION('center_axis',(1.,0.,0.));
#4275=DIRECTION('ref_axis',(0.,0.,-1.));
#4276=DIRECTION('',(0.,0.,-1.));
#4277=DIRECTION('center_axis',(0.,1.,0.));
#4278=DIRECTION('ref_axis',(0.,0.,1.));
#4279=DIRECTION('axis',(0.,0.,1.));
#4280=DIRECTION('refdir',(1.,0.,0.));
#4281=DIRECTION('center_axis',(0.,1.,0.));
#4282=DIRECTION('ref_axis',(0.,0.,1.));
#4283=DIRECTION('center_axis',(0.,-1.,0.));
#4284=DIRECTION('ref_axis',(-1.,0.,0.));
#4285=DIRECTION('center_axis',(-1.,0.,1.22464679914735E-16));
#4286=DIRECTION('ref_axis',(-1.22464679914735E-16,0.,-1.));
#4287=DIRECTION('center_axis',(0.,1.,0.));
#4288=DIRECTION('ref_axis',(-1.,0.,0.));
#4289=DIRECTION('center_axis',(0.,1.,0.));
#4290=DIRECTION('ref_axis',(-1.,0.,0.));
#4291=DIRECTION('center_axis',(0.,1.,0.));
#4292=DIRECTION('ref_axis',(-1.,0.,0.));
#4293=DIRECTION('',(0.,-1.,0.));
#4294=DIRECTION('center_axis',(0.,-1.,0.));
#4295=DIRECTION('ref_axis',(-1.,0.,0.));
#4296=DIRECTION('center_axis',(0.,-1.,0.));
#4297=DIRECTION('ref_axis',(-1.,0.,0.));
#4298=DIRECTION('center_axis',(0.,1.,0.));
#4299=DIRECTION('ref_axis',(-1.,0.,0.));
#4300=DIRECTION('center_axis',(0.,-1.,0.));
#4301=DIRECTION('ref_axis',(-1.,0.,0.));
#4302=DIRECTION('center_axis',(0.,1.,0.));
#4303=DIRECTION('ref_axis',(0.,0.,1.));
#4304=DIRECTION('center_axis',(-1.,0.,1.22464679914735E-16));
#4305=DIRECTION('ref_axis',(-1.22464679914735E-16,0.,-1.));
#4306=DIRECTION('center_axis',(0.,1.,0.));
#4307=DIRECTION('ref_axis',(-1.,0.,0.));
#4308=DIRECTION('center_axis',(0.,1.,0.));
#4309=DIRECTION('ref_axis',(-1.,0.,0.));
#4310=DIRECTION('center_axis',(0.,-1.,0.));
#4311=DIRECTION('ref_axis',(-1.,0.,0.));
#4312=DIRECTION('center_axis',(0.,1.,0.));
#4313=DIRECTION('ref_axis',(-1.,0.,0.));
#4314=DIRECTION('',(0.,-1.,0.));
#4315=DIRECTION('axis',(0.,0.,1.));
#4316=DIRECTION('refdir',(1.,0.,0.));
#4317=DIRECTION('center_axis',(0.,1.,0.));
#4318=DIRECTION('ref_axis',(1.,0.,0.));
#4319=DIRECTION('center_axis',(0.,1.,0.));
#4320=DIRECTION('ref_axis',(1.,0.,0.));
#4321=DIRECTION('',(0.,1.,0.));
#4322=DIRECTION('center_axis',(0.,-1.,0.));
#4323=DIRECTION('ref_axis',(1.,0.,0.));
#4324=DIRECTION('center_axis',(0.,1.,0.));
#4325=DIRECTION('ref_axis',(1.,0.,0.));
#4326=DIRECTION('',(-1.,0.,0.));
#4327=DIRECTION('',(0.,0.,-1.));
#4328=DIRECTION('',(1.,0.,0.));
#4329=DIRECTION('',(0.,0.,-1.));
#4330=DIRECTION('center_axis',(0.,-1.,0.));
#4331=DIRECTION('ref_axis',(-1.,0.,0.));
#4332=DIRECTION('',(1.,0.,0.));
#4333=DIRECTION('',(0.,0.,-1.));
#4334=DIRECTION('',(-1.,0.,0.));
#4335=DIRECTION('',(0.,0.,-1.));
#4336=DIRECTION('center_axis',(0.,0.,-1.));
#4337=DIRECTION('ref_axis',(-1.,0.,0.));
#4338=DIRECTION('',(0.,1.,0.));
#4339=DIRECTION('',(0.,-1.,0.));
#4340=DIRECTION('center_axis',(0.,0.,-1.));
#4341=DIRECTION('ref_axis',(-1.,0.,0.));
#4342=DIRECTION('',(0.,1.,0.));
#4343=DIRECTION('',(-1.,0.,0.));
#4344=DIRECTION('',(0.,1.,0.));
#4345=DIRECTION('center_axis',(0.,0.,-1.));
#4346=DIRECTION('ref_axis',(-1.,0.,0.));
#4347=DIRECTION('',(0.,1.,0.));
#4348=DIRECTION('',(-1.,0.,0.));
#4349=DIRECTION('',(0.,1.,0.));
#4350=DIRECTION('center_axis',(0.,0.,1.));
#4351=DIRECTION('ref_axis',(1.,0.,0.));
#4352=DIRECTION('center_axis',(0.,0.,1.));
#4353=DIRECTION('ref_axis',(-1.,0.,0.));
#4354=DIRECTION('',(0.,1.,0.));
#4355=DIRECTION('center_axis',(0.,0.,1.));
#4356=DIRECTION('ref_axis',(1.,0.,0.));
#4357=DIRECTION('center_axis',(0.,0.,1.));
#4358=DIRECTION('ref_axis',(-1.,0.,0.));
#4359=DIRECTION('center_axis',(0.,0.,1.));
#4360=DIRECTION('ref_axis',(-1.,0.,0.));
#4361=DIRECTION('',(0.,1.,0.));
#4362=DIRECTION('center_axis',(0.,0.,1.));
#4363=DIRECTION('ref_axis',(1.,0.,0.));
#4364=DIRECTION('center_axis',(0.,0.,1.));
#4365=DIRECTION('ref_axis',(-1.,0.,0.));
#4366=DIRECTION('center_axis',(0.,0.,1.));
#4367=DIRECTION('ref_axis',(-1.,0.,0.));
#4368=DIRECTION('',(0.,1.,0.));
#4369=DIRECTION('center_axis',(0.,0.,1.));
#4370=DIRECTION('ref_axis',(1.,0.,0.));
#4371=DIRECTION('center_axis',(0.,0.,1.));
#4372=DIRECTION('ref_axis',(-1.,0.,0.));
#4373=DIRECTION('',(0.,1.,0.));
#4374=DIRECTION('center_axis',(1.,0.,0.));
#4375=DIRECTION('ref_axis',(0.,0.,-1.));
#4376=DIRECTION('',(0.,0.,-1.));
#4377=DIRECTION('',(0.,0.,-1.));
#4378=DIRECTION('',(0.,1.,0.));
#4379=DIRECTION('',(0.,1.,0.));
#4380=DIRECTION('',(0.,1.,0.));
#4381=DIRECTION('center_axis',(-1.,0.,0.));
#4382=DIRECTION('ref_axis',(0.,0.,1.));
#4383=DIRECTION('',(0.,0.,1.));
#4384=DIRECTION('',(0.,-1.,0.));
#4385=DIRECTION('',(0.,-1.,0.));
#4386=DIRECTION('',(0.,-1.,0.));
#4387=DIRECTION('',(0.,0.,1.));
#4388=DIRECTION('center_axis',(0.,0.,-1.));
#4389=DIRECTION('ref_axis',(1.,0.,0.));
#4390=DIRECTION('center_axis',(0.,0.,1.));
#4391=DIRECTION('ref_axis',(-1.,0.,0.));
#4392=DIRECTION('center_axis',(0.,0.,1.));
#4393=DIRECTION('ref_axis',(-1.,0.,0.));
#4394=DIRECTION('',(-1.,0.,-8.88178419700125E-17));
#4395=DIRECTION('',(0.,-1.,0.));
#4396=DIRECTION('',(1.,0.,0.));
#4397=DIRECTION('center_axis',(0.,0.,-1.));
#4398=DIRECTION('ref_axis',(1.,0.,0.));
#4399=DIRECTION('',(1.,0.,0.));
#4400=DIRECTION('',(0.,-1.,0.));
#4401=DIRECTION('',(-1.,0.,-8.88178419700125E-17));
#4402=DIRECTION('center_axis',(0.,0.,1.));
#4403=DIRECTION('ref_axis',(-1.,0.,0.));
#4404=DIRECTION('center_axis',(0.,0.,1.));
#4405=DIRECTION('ref_axis',(-1.,0.,0.));
#4406=DIRECTION('center_axis',(0.,0.,1.));
#4407=DIRECTION('ref_axis',(-1.,0.,0.));
#4408=DIRECTION('center_axis',(0.,0.,1.));
#4409=DIRECTION('ref_axis',(-1.,0.,0.));
#4410=DIRECTION('center_axis',(0.,0.,-1.));
#4411=DIRECTION('ref_axis',(-1.,0.,0.));
#4412=DIRECTION('center_axis',(0.,0.,-1.));
#4413=DIRECTION('ref_axis',(-1.,0.,0.));
#4414=DIRECTION('',(0.,0.,-1.));
#4415=DIRECTION('center_axis',(0.,0.,-1.));
#4416=DIRECTION('ref_axis',(-1.,0.,0.));
#4417=DIRECTION('center_axis',(0.,0.,-1.));
#4418=DIRECTION('ref_axis',(-1.,0.,0.));
#4419=DIRECTION('',(0.,0.,-1.));
#4420=DIRECTION('center_axis',(0.,0.,-1.));
#4421=DIRECTION('ref_axis',(-1.,0.,0.));
#4422=DIRECTION('center_axis',(0.,0.,-1.));
#4423=DIRECTION('ref_axis',(-1.,0.,0.));
#4424=DIRECTION('',(0.,0.,-1.));
#4425=DIRECTION('center_axis',(0.,0.,-1.));
#4426=DIRECTION('ref_axis',(-1.,0.,0.));
#4427=DIRECTION('center_axis',(0.,0.,-1.));
#4428=DIRECTION('ref_axis',(-1.,0.,0.));
#4429=DIRECTION('',(0.,0.,-1.));
#4430=DIRECTION('center_axis',(-1.,0.,-8.88178419700125E-17));
#4431=DIRECTION('ref_axis',(8.88178419700125E-17,0.,-1.));
#4432=DIRECTION('',(8.88178419700125E-17,0.,-1.));
#4433=DIRECTION('',(8.88178419700125E-17,0.,-1.));
#4434=DIRECTION('',(0.,-1.,0.));
#4435=DIRECTION('center_axis',(8.88178419700125E-17,0.,-1.));
#4436=DIRECTION('ref_axis',(1.,0.,8.88178419700125E-17));
#4437=DIRECTION('',(1.,0.,8.88178419700125E-17));
#4438=DIRECTION('',(1.,0.,8.88178419700125E-17));
#4439=DIRECTION('',(0.,-1.,0.));
#4440=DIRECTION('center_axis',(-1.,0.,-8.88178419700125E-17));
#4441=DIRECTION('ref_axis',(8.88178419700125E-17,0.,-1.));
#4442=DIRECTION('',(8.88178419700125E-17,0.,-1.));
#4443=DIRECTION('',(8.88178419700125E-17,0.,-1.));
#4444=DIRECTION('',(0.,-1.,0.));
#4445=DIRECTION('center_axis',(1.,0.,8.88178419700125E-17));
#4446=DIRECTION('ref_axis',(-8.88178419700125E-17,0.,1.));
#4447=DIRECTION('',(-8.88178419700125E-17,0.,1.));
#4448=DIRECTION('',(0.,-1.,0.));
#4449=DIRECTION('',(-8.88178419700125E-17,0.,1.));
#4450=DIRECTION('',(0.,-1.,0.));
#4451=DIRECTION('center_axis',(-8.88178419700125E-17,0.,1.));
#4452=DIRECTION('ref_axis',(-1.,0.,-8.88178419700125E-17));
#4453=DIRECTION('',(-1.,0.,-8.88178419700125E-17));
#4454=DIRECTION('',(-1.,0.,-8.88178419700125E-17));
#4455=DIRECTION('center_axis',(0.,-1.,0.));
#4456=DIRECTION('ref_axis',(0.,0.,-1.));
#4457=DIRECTION('',(0.,0.,-1.));
#4458=DIRECTION('',(-1.,0.,0.));
#4459=DIRECTION('',(0.,0.,-1.));
#4460=DIRECTION('',(1.,0.,8.88178419700125E-17));
#4461=DIRECTION('',(0.,0.,1.));
#4462=DIRECTION('',(1.,0.,0.));
#4463=DIRECTION('center_axis',(-1.,0.,0.));
#4464=DIRECTION('ref_axis',(0.,0.,-1.));
#4465=DIRECTION('',(0.,-1.,0.));
#4466=DIRECTION('',(0.,0.,-1.));
#4467=DIRECTION('center_axis',(0.,0.,1.));
#4468=DIRECTION('ref_axis',(-1.,0.,0.));
#4469=DIRECTION('',(0.,-1.,0.));
#4470=DIRECTION('',(-1.,0.,0.));
#4471=DIRECTION('center_axis',(-1.,0.,0.));
#4472=DIRECTION('ref_axis',(0.,0.,-1.));
#4473=DIRECTION('',(0.,-1.,0.));
#4474=DIRECTION('',(0.,0.,-1.));
#4475=DIRECTION('center_axis',(0.,0.,1.));
#4476=DIRECTION('ref_axis',(-1.,0.,0.));
#4477=DIRECTION('',(-1.,0.,0.));
#4478=DIRECTION('',(0.,-1.,0.));
#4479=DIRECTION('center_axis',(1.,0.,0.));
#4480=DIRECTION('ref_axis',(0.,0.,1.));
#4481=DIRECTION('',(0.,0.,1.));
#4482=DIRECTION('',(0.,-1.,0.));
#4483=DIRECTION('center_axis',(0.,0.,-1.));
#4484=DIRECTION('ref_axis',(1.,0.,0.));
#4485=DIRECTION('',(1.,0.,0.));
#4486=DIRECTION('center_axis',(0.,-1.,0.));
#4487=DIRECTION('ref_axis',(0.,0.,-1.));
#4488=DIRECTION('axis',(0.,0.,1.));
#4489=DIRECTION('refdir',(1.,0.,0.));
#4490=DIRECTION('center_axis',(0.,1.,0.));
#4491=DIRECTION('ref_axis',(-0.707106781186547,0.,-0.707106781186547));
#4492=DIRECTION('center_axis',(0.,-1.,0.));
#4493=DIRECTION('ref_axis',(-0.707106781186547,0.,-0.707106781186547));
#4494=DIRECTION('',(0.,-1.,0.));
#4495=DIRECTION('center_axis',(0.,1.,0.));
#4496=DIRECTION('ref_axis',(-0.707106781186547,0.,-0.707106781186547));
#4497=DIRECTION('',(0.,1.,0.));
#4498=DIRECTION('center_axis',(0.,1.,0.));
#4499=DIRECTION('ref_axis',(-1.,0.,0.));
#4500=DIRECTION('',(-1.,0.,0.));
#4501=DIRECTION('center_axis',(0.,1.,0.));
#4502=DIRECTION('ref_axis',(0.707106781186547,0.,-0.707106781186547));
#4503=DIRECTION('',(0.,0.,-1.));
#4504=DIRECTION('center_axis',(0.,1.,0.));
#4505=DIRECTION('ref_axis',(0.707106781186547,0.,0.707106781186547));
#4506=DIRECTION('',(1.,0.,0.));
#4507=DIRECTION('center_axis',(0.,1.,0.));
#4508=DIRECTION('ref_axis',(-0.707106781186547,0.,0.707106781186547));
#4509=DIRECTION('',(0.,0.,1.));
#4510=DIRECTION('center_axis',(0.,0.,-1.));
#4511=DIRECTION('ref_axis',(-1.,0.,0.));
#4512=DIRECTION('',(-1.,0.,0.));
#4513=DIRECTION('',(0.,1.,0.));
#4514=DIRECTION('center_axis',(0.,1.,0.));
#4515=DIRECTION('ref_axis',(0.707106781186547,0.,-0.707106781186547));
#4516=DIRECTION('center_axis',(0.,-1.,0.));
#4517=DIRECTION('ref_axis',(0.707106781186547,0.,-0.707106781186547));
#4518=DIRECTION('',(0.,-1.,0.));
#4519=DIRECTION('center_axis',(0.,1.,0.));
#4520=DIRECTION('ref_axis',(-0.707106781186547,0.,0.707106781186547));
#4521=DIRECTION('center_axis',(0.,-1.,0.));
#4522=DIRECTION('ref_axis',(-0.707106781186547,0.,0.707106781186547));
#4523=DIRECTION('',(0.,-1.,0.));
#4524=DIRECTION('',(0.,1.,0.));
#4525=DIRECTION('center_axis',(0.,0.,1.));
#4526=DIRECTION('ref_axis',(1.,0.,0.));
#4527=DIRECTION('',(0.,-1.,0.));
#4528=DIRECTION('',(1.,0.,0.));
#4529=DIRECTION('center_axis',(0.,1.,0.));
#4530=DIRECTION('ref_axis',(0.707106781186547,0.,0.707106781186547));
#4531=DIRECTION('center_axis',(0.,-1.,0.));
#4532=DIRECTION('ref_axis',(0.707106781186547,0.,0.707106781186547));
#4533=DIRECTION('',(0.,1.,0.));
#4534=DIRECTION('center_axis',(1.,0.,0.));
#4535=DIRECTION('ref_axis',(0.,0.,-1.));
#4536=DIRECTION('',(0.,0.,-1.));
#4537=DIRECTION('center_axis',(-1.,0.,0.));
#4538=DIRECTION('ref_axis',(0.,0.,1.));
#4539=DIRECTION('',(0.,0.,1.));
#4540=DIRECTION('center_axis',(0.,1.,0.));
#4541=DIRECTION('ref_axis',(0.,0.,1.));
#4542=DIRECTION('axis',(0.,0.,1.));
#4543=DIRECTION('refdir',(1.,0.,0.));
#4544=DIRECTION('center_axis',(0.,1.,0.));
#4545=DIRECTION('ref_axis',(-1.,0.,0.));
#4546=DIRECTION('center_axis',(0.,1.,0.));
#4547=DIRECTION('ref_axis',(-1.,0.,0.));
#4548=DIRECTION('',(0.,-1.,0.));
#4549=DIRECTION('center_axis',(0.,-1.,0.));
#4550=DIRECTION('ref_axis',(-1.,0.,0.));
#4551=DIRECTION('center_axis',(0.,1.,0.));
#4552=DIRECTION('ref_axis',(-1.,0.,0.));
#4553=DIRECTION('center_axis',(0.,-1.,0.));
#4554=DIRECTION('ref_axis',(-1.,0.,0.));
#4555=DIRECTION('center_axis',(0.,-1.,0.));
#4556=DIRECTION('ref_axis',(-1.,0.,0.));
#4557=DIRECTION('',(0.,1.,0.));
#4558=DIRECTION('center_axis',(0.,-1.,0.));
#4559=DIRECTION('ref_axis',(-1.,0.,0.));
#4560=DIRECTION('center_axis',(0.,1.,0.));
#4561=DIRECTION('ref_axis',(-1.,0.,0.));
#4562=DIRECTION('center_axis',(0.,1.,0.));
#4563=DIRECTION('ref_axis',(-1.,0.,0.));
#4564=DIRECTION('axis',(0.,0.,1.));
#4565=DIRECTION('refdir',(1.,0.,0.));
#4566=DIRECTION('center_axis',(0.,-1.,0.));
#4567=DIRECTION('ref_axis',(-1.,0.,0.));
#4568=DIRECTION('center_axis',(0.,-1.,0.));
#4569=DIRECTION('ref_axis',(-1.,0.,0.));
#4570=DIRECTION('',(0.,-1.,0.));
#4571=DIRECTION('center_axis',(0.,1.,0.));
#4572=DIRECTION('ref_axis',(-1.,0.,0.));
#4573=DIRECTION('center_axis',(0.,1.,0.));
#4574=DIRECTION('ref_axis',(1.,0.,0.));
#4575=DIRECTION('',(1.,0.,0.));
#4576=DIRECTION('',(0.,0.,-1.));
#4577=DIRECTION('',(-1.,0.,0.));
#4578=DIRECTION('',(0.,0.,-1.));
#4579=DIRECTION('center_axis',(-1.,7.40148683083438E-17,0.));
#4580=DIRECTION('ref_axis',(7.40148683083438E-17,1.,0.));
#4581=DIRECTION('',(7.40148683083438E-17,1.,0.));
#4582=DIRECTION('',(0.,0.,-1.));
#4583=DIRECTION('',(-7.40148683083438E-17,-1.,0.));
#4584=DIRECTION('center_axis',(0.,-1.,0.));
#4585=DIRECTION('ref_axis',(-1.,0.,0.));
#4586=DIRECTION('',(-1.,0.,0.));
#4587=DIRECTION('',(0.,0.,-1.));
#4588=DIRECTION('',(1.,0.,0.));
#4589=DIRECTION('center_axis',(1.,7.40148683083438E-17,0.));
#4590=DIRECTION('ref_axis',(7.40148683083438E-17,-1.,0.));
#4591=DIRECTION('',(7.40148683083438E-17,-1.,0.));
#4592=DIRECTION('',(-7.40148683083438E-17,1.,0.));
#4593=DIRECTION('center_axis',(0.707106781186548,0.,-0.707106781186548));
#4594=DIRECTION('ref_axis',(-0.707106781186548,0.,-0.707106781186548));
#4595=DIRECTION('',(0.707106781186548,0.,0.707106781186548));
#4596=DIRECTION('',(0.,-1.,0.));
#4597=DIRECTION('',(-0.707106781186548,0.,-0.707106781186548));
#4598=DIRECTION('',(0.,1.,0.));
#4599=DIRECTION('center_axis',(0.,0.,-1.));
#4600=DIRECTION('ref_axis',(-1.,0.,0.));
#4601=DIRECTION('',(-1.,0.,0.));
#4602=DIRECTION('',(0.,-1.,0.));
#4603=DIRECTION('',(-1.,0.,0.));
#4604=DIRECTION('center_axis',(0.,1.,0.));
#4605=DIRECTION('ref_axis',(-1.,0.,0.));
#4606=DIRECTION('',(0.,0.,1.));
#4607=DIRECTION('',(0.707106781186548,0.,-0.707106781186548));
#4608=DIRECTION('',(-1.,0.,0.));
#4609=DIRECTION('',(0.707106781186548,0.,0.707106781186548));
#4610=DIRECTION('',(0.,0.,-1.));
#4611=DIRECTION('',(-0.707106781186548,0.,0.707106781186548));
#4612=DIRECTION('center_axis',(0.707106781186548,0.,0.707106781186548));
#4613=DIRECTION('ref_axis',(0.707106781186548,0.,-0.707106781186548));
#4614=DIRECTION('',(-0.707106781186548,0.,0.707106781186548));
#4615=DIRECTION('',(0.,-1.,0.));
#4616=DIRECTION('',(0.,1.,0.));
#4617=DIRECTION('center_axis',(0.,0.,1.));
#4618=DIRECTION('ref_axis',(1.,0.,0.));
#4619=DIRECTION('',(1.,0.,0.));
#4620=DIRECTION('',(0.,1.,0.));
#4621=DIRECTION('center_axis',(-0.707106781186548,0.,0.707106781186548));
#4622=DIRECTION('ref_axis',(0.707106781186548,0.,0.707106781186548));
#4623=DIRECTION('',(-0.707106781186548,0.,-0.707106781186548));
#4624=DIRECTION('',(0.,-1.,0.));
#4625=DIRECTION('center_axis',(-0.707106781186548,0.,-0.707106781186548));
#4626=DIRECTION('ref_axis',(-0.707106781186548,0.,0.707106781186548));
#4627=DIRECTION('',(0.707106781186548,0.,-0.707106781186548));
#4628=DIRECTION('',(0.,1.,0.));
#4629=DIRECTION('center_axis',(-1.,0.,0.));
#4630=DIRECTION('ref_axis',(0.,0.,1.));
#4631=DIRECTION('',(0.,0.,1.));
#4632=DIRECTION('center_axis',(1.,0.,0.));
#4633=DIRECTION('ref_axis',(0.,0.,-1.));
#4634=DIRECTION('',(0.,0.,-1.));
#4635=DIRECTION('center_axis',(0.,1.,0.));
#4636=DIRECTION('ref_axis',(0.,0.,1.));
#4637=DIRECTION('axis',(0.,0.,1.));
#4638=DIRECTION('refdir',(1.,0.,0.));
#4639=DIRECTION('center_axis',(0.,-1.,0.));
#4640=DIRECTION('ref_axis',(0.,0.,-1.));
#4641=DIRECTION('center_axis',(0.,-1.,0.));
#4642=DIRECTION('ref_axis',(0.,0.,1.));
#4643=DIRECTION('center_axis',(-1.,0.,-1.22464679914735E-16));
#4644=DIRECTION('ref_axis',(-1.22464679914735E-16,0.,1.));
#4645=DIRECTION('center_axis',(0.,1.,0.));
#4646=DIRECTION('ref_axis',(0.,0.,1.));
#4647=DIRECTION('center_axis',(0.,-1.,0.));
#4648=DIRECTION('ref_axis',(0.,0.,-1.));
#4649=DIRECTION('center_axis',(0.,-1.,0.));
#4650=DIRECTION('ref_axis',(0.,0.,1.));
#4651=DIRECTION('',(0.,1.,0.));
#4652=DIRECTION('center_axis',(0.,-1.,0.));
#4653=DIRECTION('ref_axis',(0.,0.,-1.));
#4654=DIRECTION('center_axis',(0.,1.,0.));
#4655=DIRECTION('ref_axis',(1.20388952477896E-16,0.,1.));
#4656=DIRECTION('center_axis',(0.,-1.,0.));
#4657=DIRECTION('ref_axis',(0.,0.,-1.));
#4658=DIRECTION('center_axis',(0.,-1.,0.));
#4659=DIRECTION('ref_axis',(0.,0.,1.));
#4660=DIRECTION('center_axis',(-1.,0.,-1.22464679914735E-16));
#4661=DIRECTION('ref_axis',(-1.22464679914735E-16,0.,1.));
#4662=DIRECTION('center_axis',(0.,1.,0.));
#4663=DIRECTION('ref_axis',(0.,0.,1.));
#4664=DIRECTION('center_axis',(0.,-1.,0.));
#4665=DIRECTION('ref_axis',(0.,0.,-1.));
#4666=DIRECTION('center_axis',(0.,-1.,0.));
#4667=DIRECTION('ref_axis',(0.,0.,1.));
#4668=DIRECTION('',(0.,1.,0.));
#4669=DIRECTION('center_axis',(0.,-1.,0.));
#4670=DIRECTION('ref_axis',(0.,0.,-1.));
#4671=DIRECTION('center_axis',(0.,1.,0.));
#4672=DIRECTION('ref_axis',(0.,0.,1.));
#4673=DIRECTION('center_axis',(0.,-1.,0.));
#4674=DIRECTION('ref_axis',(0.,0.,-1.));
#4675=DIRECTION('center_axis',(0.,1.,0.));
#4676=DIRECTION('ref_axis',(0.,0.,1.));
#4677=DIRECTION('center_axis',(-1.,0.,-1.22464679914735E-16));
#4678=DIRECTION('ref_axis',(-1.22464679914735E-16,0.,1.));
#4679=DIRECTION('center_axis',(0.,-1.,0.));
#4680=DIRECTION('ref_axis',(0.,0.,-1.));
#4681=DIRECTION('center_axis',(0.,-1.,0.));
#4682=DIRECTION('ref_axis',(0.,0.,-1.));
#4683=DIRECTION('center_axis',(-1.,0.,-1.22464679914735E-16));
#4684=DIRECTION('ref_axis',(-1.22464679914735E-16,0.,1.));
#4685=DIRECTION('center_axis',(0.,-1.,0.));
#4686=DIRECTION('ref_axis',(0.,0.,-1.));
#4687=DIRECTION('center_axis',(-1.,0.,-1.22464679914735E-16));
#4688=DIRECTION('ref_axis',(-1.22464679914735E-16,0.,1.));
#4689=DIRECTION('center_axis',(0.,-1.,0.));
#4690=DIRECTION('ref_axis',(1.20388952477896E-16,0.,1.));
#4691=DIRECTION('center_axis',(0.,-1.,0.));
#4692=DIRECTION('ref_axis',(0.,0.,-1.));
#4693=DIRECTION('',(0.,1.,0.));
#4694=DIRECTION('center_axis',(0.,-1.,0.));
#4695=DIRECTION('ref_axis',(1.,0.,0.));
#4696=DIRECTION('center_axis',(0.,1.,0.));
#4697=DIRECTION('ref_axis',(0.,0.,1.));
#4698=DIRECTION('axis',(0.,0.,1.));
#4699=DIRECTION('refdir',(1.,0.,0.));
#4700=DIRECTION('center_axis',(0.,-1.,0.));
#4701=DIRECTION('ref_axis',(1.,0.,0.));
#4702=DIRECTION('center_axis',(0.,1.,0.));
#4703=DIRECTION('ref_axis',(1.,0.,0.));
#4704=DIRECTION('',(0.,1.,0.));
#4705=DIRECTION('center_axis',(0.,1.,0.));
#4706=DIRECTION('ref_axis',(1.,0.,0.));
#4707=DIRECTION('center_axis',(0.,-1.,0.));
#4708=DIRECTION('ref_axis',(1.,0.,0.));
#4709=DIRECTION('center_axis',(0.,1.,0.));
#4710=DIRECTION('ref_axis',(1.,0.,0.));
#4711=DIRECTION('',(0.,1.,0.));
#4712=DIRECTION('center_axis',(0.,1.,0.));
#4713=DIRECTION('ref_axis',(1.,0.,0.));
#4714=DIRECTION('center_axis',(0.,-1.,0.));
#4715=DIRECTION('ref_axis',(1.,0.,0.));
#4716=DIRECTION('center_axis',(0.,1.,0.));
#4717=DIRECTION('ref_axis',(1.,0.,0.));
#4718=DIRECTION('',(0.,1.,0.));
#4719=DIRECTION('center_axis',(0.,1.,0.));
#4720=DIRECTION('ref_axis',(1.,0.,0.));
#4721=DIRECTION('center_axis',(0.,-1.,0.));
#4722=DIRECTION('ref_axis',(1.,0.,0.));
#4723=DIRECTION('center_axis',(0.,1.,0.));
#4724=DIRECTION('ref_axis',(1.,0.,0.));
#4725=DIRECTION('',(0.,1.,0.));
#4726=DIRECTION('center_axis',(0.,1.,0.));
#4727=DIRECTION('ref_axis',(1.,0.,0.));
#4728=DIRECTION('center_axis',(0.,0.,-1.));
#4729=DIRECTION('ref_axis',(1.,0.,0.));
#4730=DIRECTION('',(1.,0.,0.));
#4731=DIRECTION('',(0.,-1.,0.));
#4732=DIRECTION('',(1.,0.,0.));
#4733=DIRECTION('',(0.,-1.,0.));
#4734=DIRECTION('center_axis',(1.,0.,0.));
#4735=DIRECTION('ref_axis',(0.,0.,1.));
#4736=DIRECTION('',(0.,0.,1.));
#4737=DIRECTION('',(0.,0.,1.));
#4738=DIRECTION('',(0.,-1.,0.));
#4739=DIRECTION('center_axis',(0.,0.,1.));
#4740=DIRECTION('ref_axis',(-1.,0.,0.));
#4741=DIRECTION('',(-1.,0.,0.));
#4742=DIRECTION('',(-1.,0.,0.));
#4743=DIRECTION('',(0.,-1.,0.));
#4744=DIRECTION('center_axis',(1.,0.,0.));
#4745=DIRECTION('ref_axis',(0.,0.,1.));
#4746=DIRECTION('',(0.,0.,1.));
#4747=DIRECTION('',(0.,0.,1.));
#4748=DIRECTION('',(0.,-1.,0.));
#4749=DIRECTION('center_axis',(0.,0.,-1.));
#4750=DIRECTION('ref_axis',(1.,0.,0.));
#4751=DIRECTION('',(1.,0.,0.));
#4752=DIRECTION('',(1.,0.,0.));
#4753=DIRECTION('',(0.,-1.,0.));
#4754=DIRECTION('center_axis',(-1.,0.,0.));
#4755=DIRECTION('ref_axis',(0.,0.,-1.));
#4756=DIRECTION('',(0.,0.,-1.));
#4757=DIRECTION('',(0.,0.,-1.));
#4758=DIRECTION('',(0.,-1.,0.));
#4759=DIRECTION('center_axis',(0.,0.,1.));
#4760=DIRECTION('ref_axis',(-1.,0.,0.));
#4761=DIRECTION('',(-1.,0.,0.));
#4762=DIRECTION('',(-1.,0.,0.));
#4763=DIRECTION('',(0.,-1.,0.));
#4764=DIRECTION('center_axis',(1.,0.,0.));
#4765=DIRECTION('ref_axis',(0.,0.,1.));
#4766=DIRECTION('',(0.,0.,1.));
#4767=DIRECTION('',(0.,0.,1.));
#4768=DIRECTION('',(0.,-1.,0.));
#4769=DIRECTION('center_axis',(0.,0.,-1.));
#4770=DIRECTION('ref_axis',(1.,0.,0.));
#4771=DIRECTION('',(1.,0.,0.));
#4772=DIRECTION('',(1.,0.,0.));
#4773=DIRECTION('',(0.,-1.,0.));
#4774=DIRECTION('center_axis',(-1.,0.,0.));
#4775=DIRECTION('ref_axis',(0.,0.,-1.));
#4776=DIRECTION('',(0.,0.,-1.));
#4777=DIRECTION('',(0.,0.,-1.));
#4778=DIRECTION('center_axis',(0.,-1.,0.));
#4779=DIRECTION('ref_axis',(1.,0.,0.));
#4780=DIRECTION('center_axis',(0.,-1.,0.));
#4781=DIRECTION('ref_axis',(1.,0.,0.));
#4782=DIRECTION('axis',(0.,0.,1.));
#4783=DIRECTION('refdir',(1.,0.,0.));
#4784=DIRECTION('center_axis',(0.,1.,0.));
#4785=DIRECTION('ref_axis',(-1.,0.,0.));
#4786=DIRECTION('center_axis',(0.,-1.,0.));
#4787=DIRECTION('ref_axis',(-1.,0.,0.));
#4788=DIRECTION('',(0.,1.,0.));
#4789=DIRECTION('center_axis',(0.,-1.,0.));
#4790=DIRECTION('ref_axis',(-1.,0.,0.));
#4791=DIRECTION('center_axis',(0.,1.,0.));
#4792=DIRECTION('ref_axis',(-1.,0.,0.));
#4793=DIRECTION('center_axis',(0.,-1.,0.));
#4794=DIRECTION('ref_axis',(-1.,0.,0.));
#4795=DIRECTION('',(0.,1.,0.));
#4796=DIRECTION('center_axis',(0.,-1.,0.));
#4797=DIRECTION('ref_axis',(-1.,0.,0.));
#4798=DIRECTION('center_axis',(0.,1.,0.));
#4799=DIRECTION('ref_axis',(-1.,0.,0.));
#4800=DIRECTION('center_axis',(0.,-1.,0.));
#4801=DIRECTION('ref_axis',(-1.,0.,0.));
#4802=DIRECTION('',(0.,1.,0.));
#4803=DIRECTION('center_axis',(0.,-1.,0.));
#4804=DIRECTION('ref_axis',(-1.,0.,0.));
#4805=DIRECTION('center_axis',(0.,1.,0.));
#4806=DIRECTION('ref_axis',(-1.,0.,0.));
#4807=DIRECTION('center_axis',(0.,-1.,0.));
#4808=DIRECTION('ref_axis',(-1.,0.,0.));
#4809=DIRECTION('',(0.,1.,0.));
#4810=DIRECTION('center_axis',(0.,-1.,0.));
#4811=DIRECTION('ref_axis',(-1.,0.,0.));
#4812=DIRECTION('center_axis',(0.,0.,1.));
#4813=DIRECTION('ref_axis',(-1.,0.,0.));
#4814=DIRECTION('',(-1.,0.,0.));
#4815=DIRECTION('',(0.,-1.,0.));
#4816=DIRECTION('',(-1.,0.,0.));
#4817=DIRECTION('',(0.,-1.,0.));
#4818=DIRECTION('center_axis',(1.,0.,0.));
#4819=DIRECTION('ref_axis',(0.,0.,1.));
#4820=DIRECTION('',(0.,0.,1.));
#4821=DIRECTION('',(0.,-1.,0.));
#4822=DIRECTION('',(0.,0.,1.));
#4823=DIRECTION('center_axis',(0.,0.,-1.));
#4824=DIRECTION('ref_axis',(1.,0.,0.));
#4825=DIRECTION('',(1.,0.,0.));
#4826=DIRECTION('',(0.,-1.,0.));
#4827=DIRECTION('',(1.,0.,0.));
#4828=DIRECTION('center_axis',(1.,0.,0.));
#4829=DIRECTION('ref_axis',(0.,0.,1.));
#4830=DIRECTION('',(0.,0.,1.));
#4831=DIRECTION('',(0.,-1.,0.));
#4832=DIRECTION('',(0.,0.,1.));
#4833=DIRECTION('center_axis',(0.,0.,1.));
#4834=DIRECTION('ref_axis',(-1.,0.,0.));
#4835=DIRECTION('',(-1.,0.,0.));
#4836=DIRECTION('',(0.,-1.,0.));
#4837=DIRECTION('',(-1.,0.,0.));
#4838=DIRECTION('center_axis',(-1.,0.,0.));
#4839=DIRECTION('ref_axis',(0.,0.,-1.));
#4840=DIRECTION('',(0.,0.,-1.));
#4841=DIRECTION('',(0.,-1.,0.));
#4842=DIRECTION('',(0.,0.,-1.));
#4843=DIRECTION('center_axis',(0.,0.,-1.));
#4844=DIRECTION('ref_axis',(1.,0.,0.));
#4845=DIRECTION('',(1.,0.,0.));
#4846=DIRECTION('',(0.,-1.,0.));
#4847=DIRECTION('',(1.,0.,0.));
#4848=DIRECTION('center_axis',(1.,0.,0.));
#4849=DIRECTION('ref_axis',(0.,0.,1.));
#4850=DIRECTION('',(0.,0.,1.));
#4851=DIRECTION('',(0.,-1.,0.));
#4852=DIRECTION('',(0.,0.,1.));
#4853=DIRECTION('center_axis',(0.,0.,1.));
#4854=DIRECTION('ref_axis',(-1.,0.,0.));
#4855=DIRECTION('',(-1.,0.,0.));
#4856=DIRECTION('',(0.,-1.,0.));
#4857=DIRECTION('',(-1.,0.,0.));
#4858=DIRECTION('center_axis',(-1.,0.,0.));
#4859=DIRECTION('ref_axis',(0.,0.,-1.));
#4860=DIRECTION('',(0.,0.,-1.));
#4861=DIRECTION('',(0.,0.,-1.));
#4862=DIRECTION('center_axis',(0.,1.,0.));
#4863=DIRECTION('ref_axis',(-1.,0.,0.));
#4864=DIRECTION('center_axis',(0.,1.,0.));
#4865=DIRECTION('ref_axis',(-1.,0.,0.));
#4866=DIRECTION('axis',(0.,0.,1.));
#4867=DIRECTION('refdir',(1.,0.,0.));
#4868=DIRECTION('center_axis',(0.,-1.,0.));
#4869=DIRECTION('ref_axis',(1.,0.,0.));
#4870=DIRECTION('center_axis',(0.,1.,0.));
#4871=DIRECTION('ref_axis',(1.,0.,0.));
#4872=DIRECTION('',(0.,-1.,0.));
#4873=DIRECTION('center_axis',(0.,1.,0.));
#4874=DIRECTION('ref_axis',(1.,0.,0.));
#4875=DIRECTION('center_axis',(0.,-1.,0.));
#4876=DIRECTION('ref_axis',(1.,0.,0.));
#4877=DIRECTION('center_axis',(0.,1.,0.));
#4878=DIRECTION('ref_axis',(1.,0.,0.));
#4879=DIRECTION('',(0.,-1.,0.));
#4880=DIRECTION('center_axis',(0.,1.,0.));
#4881=DIRECTION('ref_axis',(1.,0.,0.));
#4882=DIRECTION('center_axis',(0.,-1.,0.));
#4883=DIRECTION('ref_axis',(1.,0.,0.));
#4884=DIRECTION('center_axis',(0.,1.,0.));
#4885=DIRECTION('ref_axis',(1.,0.,0.));
#4886=DIRECTION('',(0.,-1.,0.));
#4887=DIRECTION('center_axis',(0.,1.,0.));
#4888=DIRECTION('ref_axis',(1.,0.,0.));
#4889=DIRECTION('center_axis',(0.,-1.,0.));
#4890=DIRECTION('ref_axis',(1.,0.,0.));
#4891=DIRECTION('center_axis',(0.,1.,0.));
#4892=DIRECTION('ref_axis',(1.,0.,0.));
#4893=DIRECTION('',(0.,-1.,0.));
#4894=DIRECTION('center_axis',(0.,1.,0.));
#4895=DIRECTION('ref_axis',(1.,0.,0.));
#4896=DIRECTION('center_axis',(0.,0.,1.));
#4897=DIRECTION('ref_axis',(1.,0.,0.));
#4898=DIRECTION('',(1.,0.,0.));
#4899=DIRECTION('',(0.,1.,0.));
#4900=DIRECTION('',(1.,0.,0.));
#4901=DIRECTION('',(0.,1.,0.));
#4902=DIRECTION('center_axis',(-1.,0.,0.));
#4903=DIRECTION('ref_axis',(0.,0.,1.));
#4904=DIRECTION('',(0.,0.,1.));
#4905=DIRECTION('',(0.,1.,0.));
#4906=DIRECTION('',(0.,0.,1.));
#4907=DIRECTION('center_axis',(0.,0.,-1.));
#4908=DIRECTION('ref_axis',(-1.,0.,0.));
#4909=DIRECTION('',(-1.,0.,0.));
#4910=DIRECTION('',(0.,1.,0.));
#4911=DIRECTION('',(-1.,0.,0.));
#4912=DIRECTION('center_axis',(-1.,0.,0.));
#4913=DIRECTION('ref_axis',(0.,0.,1.));
#4914=DIRECTION('',(0.,0.,1.));
#4915=DIRECTION('',(0.,1.,0.));
#4916=DIRECTION('',(0.,0.,1.));
#4917=DIRECTION('center_axis',(0.,0.,1.));
#4918=DIRECTION('ref_axis',(1.,0.,0.));
#4919=DIRECTION('',(1.,0.,0.));
#4920=DIRECTION('',(0.,1.,0.));
#4921=DIRECTION('',(1.,0.,0.));
#4922=DIRECTION('center_axis',(1.,0.,0.));
#4923=DIRECTION('ref_axis',(0.,0.,-1.));
#4924=DIRECTION('',(0.,0.,-1.));
#4925=DIRECTION('',(0.,1.,0.));
#4926=DIRECTION('',(0.,0.,-1.));
#4927=DIRECTION('center_axis',(0.,0.,-1.));
#4928=DIRECTION('ref_axis',(-1.,0.,0.));
#4929=DIRECTION('',(-1.,0.,0.));
#4930=DIRECTION('',(0.,1.,0.));
#4931=DIRECTION('',(-1.,0.,0.));
#4932=DIRECTION('center_axis',(-1.,0.,0.));
#4933=DIRECTION('ref_axis',(0.,0.,1.));
#4934=DIRECTION('',(0.,0.,1.));
#4935=DIRECTION('',(0.,1.,0.));
#4936=DIRECTION('',(0.,0.,1.));
#4937=DIRECTION('center_axis',(0.,0.,1.));
#4938=DIRECTION('ref_axis',(1.,0.,0.));
#4939=DIRECTION('',(1.,0.,0.));
#4940=DIRECTION('',(0.,1.,0.));
#4941=DIRECTION('',(1.,0.,0.));
#4942=DIRECTION('center_axis',(1.,0.,0.));
#4943=DIRECTION('ref_axis',(0.,0.,-1.));
#4944=DIRECTION('',(0.,0.,-1.));
#4945=DIRECTION('',(0.,0.,-1.));
#4946=DIRECTION('center_axis',(0.,-1.,0.));
#4947=DIRECTION('ref_axis',(1.,0.,0.));
#4948=DIRECTION('center_axis',(0.,-1.,0.));
#4949=DIRECTION('ref_axis',(1.,0.,0.));
#4950=DIRECTION('axis',(0.,0.,1.));
#4951=DIRECTION('refdir',(1.,0.,0.));
#4952=DIRECTION('center_axis',(0.,1.,0.));
#4953=DIRECTION('ref_axis',(-1.,0.,0.));
#4954=DIRECTION('center_axis',(0.,-1.,0.));
#4955=DIRECTION('ref_axis',(-1.,0.,0.));
#4956=DIRECTION('',(0.,-1.,0.));
#4957=DIRECTION('center_axis',(0.,-1.,0.));
#4958=DIRECTION('ref_axis',(-1.,0.,0.));
#4959=DIRECTION('center_axis',(0.,1.,0.));
#4960=DIRECTION('ref_axis',(-1.,0.,0.));
#4961=DIRECTION('center_axis',(0.,-1.,0.));
#4962=DIRECTION('ref_axis',(-1.,0.,0.));
#4963=DIRECTION('',(0.,-1.,0.));
#4964=DIRECTION('center_axis',(0.,-1.,0.));
#4965=DIRECTION('ref_axis',(-1.,0.,0.));
#4966=DIRECTION('center_axis',(0.,1.,0.));
#4967=DIRECTION('ref_axis',(-1.,0.,0.));
#4968=DIRECTION('center_axis',(0.,-1.,0.));
#4969=DIRECTION('ref_axis',(-1.,0.,0.));
#4970=DIRECTION('',(0.,-1.,0.));
#4971=DIRECTION('center_axis',(0.,-1.,0.));
#4972=DIRECTION('ref_axis',(-1.,0.,0.));
#4973=DIRECTION('center_axis',(0.,1.,0.));
#4974=DIRECTION('ref_axis',(-1.,0.,0.));
#4975=DIRECTION('center_axis',(0.,-1.,0.));
#4976=DIRECTION('ref_axis',(-1.,0.,0.));
#4977=DIRECTION('',(0.,-1.,0.));
#4978=DIRECTION('center_axis',(0.,-1.,0.));
#4979=DIRECTION('ref_axis',(-1.,0.,0.));
#4980=DIRECTION('center_axis',(0.,0.,-1.));
#4981=DIRECTION('ref_axis',(-1.,0.,0.));
#4982=DIRECTION('',(-1.,0.,0.));
#4983=DIRECTION('',(0.,1.,0.));
#4984=DIRECTION('',(-1.,0.,0.));
#4985=DIRECTION('',(0.,1.,0.));
#4986=DIRECTION('center_axis',(-1.,0.,0.));
#4987=DIRECTION('ref_axis',(0.,0.,1.));
#4988=DIRECTION('',(0.,0.,1.));
#4989=DIRECTION('',(0.,0.,1.));
#4990=DIRECTION('',(0.,1.,0.));
#4991=DIRECTION('center_axis',(0.,0.,1.));
#4992=DIRECTION('ref_axis',(1.,0.,0.));
#4993=DIRECTION('',(1.,0.,0.));
#4994=DIRECTION('',(1.,0.,0.));
#4995=DIRECTION('',(0.,1.,0.));
#4996=DIRECTION('center_axis',(-1.,0.,0.));
#4997=DIRECTION('ref_axis',(0.,0.,1.));
#4998=DIRECTION('',(0.,0.,1.));
#4999=DIRECTION('',(0.,0.,1.));
#5000=DIRECTION('',(0.,1.,0.));
#5001=DIRECTION('center_axis',(0.,0.,-1.));
#5002=DIRECTION('ref_axis',(-1.,0.,0.));
#5003=DIRECTION('',(-1.,0.,0.));
#5004=DIRECTION('',(-1.,0.,0.));
#5005=DIRECTION('',(0.,1.,0.));
#5006=DIRECTION('center_axis',(1.,0.,0.));
#5007=DIRECTION('ref_axis',(0.,0.,-1.));
#5008=DIRECTION('',(0.,0.,-1.));
#5009=DIRECTION('',(0.,0.,-1.));
#5010=DIRECTION('',(0.,1.,0.));
#5011=DIRECTION('center_axis',(0.,0.,1.));
#5012=DIRECTION('ref_axis',(1.,0.,0.));
#5013=DIRECTION('',(1.,0.,0.));
#5014=DIRECTION('',(1.,0.,0.));
#5015=DIRECTION('',(0.,1.,0.));
#5016=DIRECTION('center_axis',(-1.,0.,0.));
#5017=DIRECTION('ref_axis',(0.,0.,1.));
#5018=DIRECTION('',(0.,0.,1.));
#5019=DIRECTION('',(0.,0.,1.));
#5020=DIRECTION('',(0.,1.,0.));
#5021=DIRECTION('center_axis',(0.,0.,-1.));
#5022=DIRECTION('ref_axis',(-1.,0.,0.));
#5023=DIRECTION('',(-1.,0.,0.));
#5024=DIRECTION('',(-1.,0.,0.));
#5025=DIRECTION('',(0.,1.,0.));
#5026=DIRECTION('center_axis',(1.,0.,0.));
#5027=DIRECTION('ref_axis',(0.,0.,-1.));
#5028=DIRECTION('',(0.,0.,-1.));
#5029=DIRECTION('',(0.,0.,-1.));
#5030=DIRECTION('center_axis',(0.,1.,0.));
#5031=DIRECTION('ref_axis',(-1.,0.,0.));
#5032=DIRECTION('center_axis',(0.,1.,0.));
#5033=DIRECTION('ref_axis',(-1.,0.,0.));
#5034=DIRECTION('',(0.,0.,1.));
#5035=DIRECTION('',(1.,0.,0.));
#5036=DIRECTION('',(0.,0.,1.));
#5037=DIRECTION('',(1.,0.,0.));
#5038=DIRECTION('',(0.,0.,1.));
#5039=DIRECTION('',(1.,0.,0.));
#5040=DIRECTION('',(0.,0.,1.));
#5041=DIRECTION('',(1.,0.,0.));
#5042=DIRECTION('',(0.,0.,1.));
#5043=DIRECTION('',(1.,0.,0.));
#5044=DIRECTION('',(0.,0.,1.));
#5045=DIRECTION('',(1.,0.,0.));
#5046=DIRECTION('',(0.,0.,1.));
#5047=DIRECTION('',(1.,0.,0.));
#5048=DIRECTION('',(0.,0.,1.));
#5049=DIRECTION('',(1.,0.,0.));
#5050=DIRECTION('',(0.,0.,1.));
#5051=DIRECTION('',(1.,0.,0.));
#5052=DIRECTION('',(0.,0.,1.));
#5053=DIRECTION('',(1.,0.,0.));
#5054=DIRECTION('',(0.,0.,1.));
#5055=DIRECTION('',(1.,0.,0.));
#5056=CARTESIAN_POINT('',(0.,0.,0.));
#5057=CARTESIAN_POINT('',(0.,0.,0.));
#5058=CARTESIAN_POINT('Origin',(4.44089209850063E-15,525.425982185852,41.5000000000007));
#5059=CARTESIAN_POINT('',(11.,60.,41.5000000000007));
#5060=CARTESIAN_POINT('Origin',(4.44089209850063E-15,60.,41.5000000000007));
#5061=CARTESIAN_POINT('',(11.,37.,41.5000000000007));
#5062=CARTESIAN_POINT('',(11.,525.425982185852,41.5000000000007));
#5063=CARTESIAN_POINT('Origin',(4.44089209850063E-15,37.,41.5000000000007));
#5064=CARTESIAN_POINT('Origin',(4.44089209850063E-15,525.425982185852,41.5000000000007));
#5065=CARTESIAN_POINT('',(11.,505.5,41.5000000000007));
#5066=CARTESIAN_POINT('Origin',(4.44089209850063E-15,505.5,41.5000000000007));
#5067=CARTESIAN_POINT('',(11.,482.5,41.5000000000007));
#5068=CARTESIAN_POINT('',(11.,525.425982185852,41.5000000000007));
#5069=CARTESIAN_POINT('Origin',(4.44089209850063E-15,482.5,41.5000000000007));
#5070=CARTESIAN_POINT('Origin',(-114.902144094842,473.010523220612,0.));
#5071=CARTESIAN_POINT('',(-89.9999999999987,473.010523220612,1.47437617670221E-12));
#5072=CARTESIAN_POINT('',(-89.9999999999987,473.010523220612,20.0000000000015));
#5073=CARTESIAN_POINT('',(-89.9999999999987,473.010523220612,7.37188088351104E-13));
#5074=CARTESIAN_POINT('',(-79.1078754759798,473.010523220612,0.));
#5075=CARTESIAN_POINT('',(-12.4510720474206,473.010523220612,1.47437617670221E-12));
#5076=CARTESIAN_POINT('',(-79.1078754759798,473.010523220612,20.0000000000015));
#5077=CARTESIAN_POINT('',(-79.1078754759798,473.010523220612,0.));
#5078=CARTESIAN_POINT('',(-102.451072047421,473.010523220612,20.0000000000015));
#5079=CARTESIAN_POINT('Origin',(-79.1078754759798,465.395629230499,0.));
#5080=CARTESIAN_POINT('',(-79.1078754759798,457.780735240385,20.0000000000015));
#5081=CARTESIAN_POINT('Origin',(-79.1078754759798,465.395629230499,20.0000000000015));
#5082=CARTESIAN_POINT('',(-79.1078754759798,457.780735240385,0.));
#5083=CARTESIAN_POINT('Origin',(-79.1078754759798,465.395629230499,1.47437617670221E-12));
#5084=CARTESIAN_POINT('',(-79.1078754759798,457.780735240385,0.));
#5085=CARTESIAN_POINT('Origin',(-79.1078754759798,457.780735240385,0.));
#5086=CARTESIAN_POINT('',(-89.9999999999987,457.780735240385,20.0000000000015));
#5087=CARTESIAN_POINT('',(-89.9999999999987,457.780735240385,1.47437617670221E-12));
#5088=CARTESIAN_POINT('',(-89.9999999999987,457.780735240385,7.37188088351104E-13));
#5089=CARTESIAN_POINT('',(-84.5539377379897,457.780735240385,20.0000000000015));
#5090=CARTESIAN_POINT('',(5.44606226201027,457.780735240385,1.47437617670221E-12));
#5091=CARTESIAN_POINT('Origin',(-114.902144094842,85.0105232206121,0.));
#5092=CARTESIAN_POINT('',(-89.9999999999987,85.0105232206121,1.47437617670221E-12));
#5093=CARTESIAN_POINT('',(-89.9999999999987,85.0105232206121,20.0000000000015));
#5094=CARTESIAN_POINT('',(-89.9999999999987,85.0105232206121,7.37188088351104E-13));
#5095=CARTESIAN_POINT('',(-79.1078754759798,85.0105232206121,0.));
#5096=CARTESIAN_POINT('',(-12.4510720474206,85.0105232206121,1.47437617670221E-12));
#5097=CARTESIAN_POINT('',(-79.1078754759798,85.0105232206121,20.0000000000015));
#5098=CARTESIAN_POINT('',(-79.1078754759798,85.0105232206121,0.));
#5099=CARTESIAN_POINT('',(-102.451072047421,85.0105232206121,20.0000000000015));
#5100=CARTESIAN_POINT('Origin',(-79.1078754759798,77.3956292304987,0.));
#5101=CARTESIAN_POINT('',(-79.1078754759798,69.7807352403852,20.0000000000015));
#5102=CARTESIAN_POINT('Origin',(-79.1078754759798,77.3956292304987,20.0000000000015));
#5103=CARTESIAN_POINT('',(-79.1078754759798,69.7807352403852,0.));
#5104=CARTESIAN_POINT('Origin',(-79.1078754759798,77.3956292304987,1.47437617670221E-12));
#5105=CARTESIAN_POINT('',(-79.1078754759798,69.7807352403852,0.));
#5106=CARTESIAN_POINT('Origin',(-79.1078754759798,69.7807352403852,0.));
#5107=CARTESIAN_POINT('',(-89.9999999999987,69.7807352403852,20.0000000000015));
#5108=CARTESIAN_POINT('',(-89.9999999999987,69.7807352403852,1.47437617670221E-12));
#5109=CARTESIAN_POINT('',(-89.9999999999987,69.7807352403852,7.37188088351104E-13));
#5110=CARTESIAN_POINT('',(-84.5539377379893,69.7807352403852,20.0000000000015));
#5111=CARTESIAN_POINT('',(5.44606226201067,69.7807352403853,1.47437617670221E-12));
#5112=CARTESIAN_POINT('Origin',(-114.902144094842,299.010523220612,0.));
#5113=CARTESIAN_POINT('',(-89.9999999999987,299.010523220612,1.47437617670221E-12));
#5114=CARTESIAN_POINT('',(-89.9999999999987,299.010523220612,20.0000000000015));
#5115=CARTESIAN_POINT('',(-89.9999999999987,299.010523220612,7.37188088351104E-13));
#5116=CARTESIAN_POINT('',(-79.1078754759798,299.010523220612,0.));
#5117=CARTESIAN_POINT('',(-12.4510720474204,299.010523220612,1.47437617670221E-12));
#5118=CARTESIAN_POINT('',(-79.1078754759798,299.010523220612,20.0000000000015));
#5119=CARTESIAN_POINT('',(-79.1078754759798,299.010523220612,0.));
#5120=CARTESIAN_POINT('',(-102.45107204742,299.010523220612,20.0000000000015));
#5121=CARTESIAN_POINT('Origin',(-79.1078754759798,291.395629230499,0.));
#5122=CARTESIAN_POINT('',(-79.1078754759798,283.780735240385,20.0000000000015));
#5123=CARTESIAN_POINT('Origin',(-79.1078754759798,291.395629230499,20.0000000000015));
#5124=CARTESIAN_POINT('',(-79.1078754759798,283.780735240385,0.));
#5125=CARTESIAN_POINT('Origin',(-79.1078754759798,291.395629230499,1.47437617670221E-12));
#5126=CARTESIAN_POINT('',(-79.1078754759798,283.780735240385,0.));
#5127=CARTESIAN_POINT('Origin',(-79.1078754759798,283.780735240385,0.));
#5128=CARTESIAN_POINT('',(-89.9999999999987,283.780735240385,20.0000000000015));
#5129=CARTESIAN_POINT('',(-89.9999999999987,283.780735240385,1.47437617670221E-12));
#5130=CARTESIAN_POINT('',(-89.9999999999987,283.780735240385,7.37188088351104E-13));
#5131=CARTESIAN_POINT('',(-84.5539377379896,283.780735240385,20.0000000000015));
#5132=CARTESIAN_POINT('',(5.44606226201044,283.780735240385,1.47437617670221E-12));
#5133=CARTESIAN_POINT('Origin',(-89.9999999999987,0.,20.0000000000015));
#5134=CARTESIAN_POINT('',(-89.9999999999987,0.,20.0000000000015));
#5135=CARTESIAN_POINT('',(-89.9999999999987,0.,20.0000000000015));
#5136=CARTESIAN_POINT('',(-89.9999999999987,37.,20.0000000000015));
#5137=CARTESIAN_POINT('',(-89.9999999999987,0.,20.0000000000015));
#5138=CARTESIAN_POINT('',(-51.5061608111161,37.,20.0000000000015));
#5139=CARTESIAN_POINT('',(-44.9999999999988,37.,20.0000000000015));
#5140=CARTESIAN_POINT('',(-51.5061608111161,505.5,20.0000000000015));
#5141=CARTESIAN_POINT('',(-51.5061608111161,0.,20.0000000000015));
#5142=CARTESIAN_POINT('',(-89.9999999999987,505.5,20.0000000000015));
#5143=CARTESIAN_POINT('',(90.0000000000013,505.5,20.0000000000015));
#5144=CARTESIAN_POINT('',(-89.9999999999987,0.,20.0000000000015));
#5145=CARTESIAN_POINT('Origin',(-89.9999999999987,0.,1.47437617670221E-12));
#5146=CARTESIAN_POINT('',(-89.9999999999987,37.,1.47437617670221E-12));
#5147=CARTESIAN_POINT('',(-89.9999999999987,0.,1.47437617670221E-12));
#5148=CARTESIAN_POINT('',(-89.9999999999987,37.,26.2500000000015));
#5149=CARTESIAN_POINT('Origin',(-89.9999999999987,0.,1.47437617670221E-12));
#5150=CARTESIAN_POINT('',(-89.9999999999987,0.,1.47437617670221E-12));
#5151=CARTESIAN_POINT('Origin',(-89.9999999999987,0.,1.47437617670221E-12));
#5152=CARTESIAN_POINT('',(-89.9999999999987,0.,1.47437617670221E-12));
#5153=CARTESIAN_POINT('Origin',(-89.9999999999987,0.,1.47437617670221E-12));
#5154=CARTESIAN_POINT('',(-89.9999999999987,505.5,1.47437617670221E-12));
#5155=CARTESIAN_POINT('',(-89.9999999999987,505.5,20.0000000000015));
#5156=CARTESIAN_POINT('',(-89.9999999999987,0.,1.47437617670221E-12));
#5157=CARTESIAN_POINT('Origin',(114.902144094842,85.0105232206121,0.));
#5158=CARTESIAN_POINT('',(79.1078754759798,85.0105232206121,20.0000000000015));
#5159=CARTESIAN_POINT('',(90.0000000000013,85.0105232206121,20.0000000000015));
#5160=CARTESIAN_POINT('',(83.2041524529792,85.0105232206121,20.0000000000015));
#5161=CARTESIAN_POINT('',(79.1078754759798,85.0105232206121,0.));
#5162=CARTESIAN_POINT('',(79.1078754759798,85.0105232206121,0.));
#5163=CARTESIAN_POINT('',(90.0000000000013,85.0105232206121,1.47437617670221E-12));
#5164=CARTESIAN_POINT('',(102.451072047422,85.0105232206121,1.47437617670221E-12));
#5165=CARTESIAN_POINT('',(90.0000000000013,85.0105232206121,10.0000000000007));
#5166=CARTESIAN_POINT('Origin',(79.1078754759798,69.7807352403852,0.));
#5167=CARTESIAN_POINT('',(90.0000000000013,69.7807352403852,20.0000000000015));
#5168=CARTESIAN_POINT('',(79.1078754759798,69.7807352403852,20.0000000000015));
#5169=CARTESIAN_POINT('',(65.307018143548,69.7807352403852,20.0000000000015));
#5170=CARTESIAN_POINT('',(90.0000000000013,69.7807352403852,1.47437617670221E-12));
#5171=CARTESIAN_POINT('',(90.0000000000013,69.7807352403852,10.0000000000007));
#5172=CARTESIAN_POINT('',(79.1078754759798,69.7807352403852,0.));
#5173=CARTESIAN_POINT('',(84.5539377379906,69.7807352403852,1.47437617670221E-12));
#5174=CARTESIAN_POINT('',(79.1078754759798,69.7807352403852,0.));
#5175=CARTESIAN_POINT('Origin',(79.1078754759798,77.3956292304987,0.));
#5176=CARTESIAN_POINT('Origin',(79.1078754759798,77.3956292304987,20.0000000000015));
#5177=CARTESIAN_POINT('Origin',(79.1078754759798,77.3956292304987,1.47437617670221E-12));
#5178=CARTESIAN_POINT('Origin',(114.902144094842,299.010523220612,0.));
#5179=CARTESIAN_POINT('',(79.1078754759798,299.010523220612,20.0000000000015));
#5180=CARTESIAN_POINT('',(90.0000000000013,299.010523220612,20.0000000000015));
#5181=CARTESIAN_POINT('',(83.2041524529791,299.010523220612,20.0000000000015));
#5182=CARTESIAN_POINT('',(79.1078754759798,299.010523220612,0.));
#5183=CARTESIAN_POINT('',(79.1078754759798,299.010523220612,0.));
#5184=CARTESIAN_POINT('',(90.0000000000013,299.010523220612,1.47437617670221E-12));
#5185=CARTESIAN_POINT('',(102.451072047422,299.010523220612,1.47437617670221E-12));
#5186=CARTESIAN_POINT('',(90.0000000000013,299.010523220612,10.0000000000007));
#5187=CARTESIAN_POINT('Origin',(79.1078754759798,283.780735240385,0.));
#5188=CARTESIAN_POINT('',(90.0000000000013,283.780735240385,20.0000000000015));
#5189=CARTESIAN_POINT('',(79.1078754759798,283.780735240385,20.0000000000015));
#5190=CARTESIAN_POINT('',(65.3070181435482,283.780735240385,20.0000000000015));
#5191=CARTESIAN_POINT('',(90.0000000000013,283.780735240385,1.47437617670221E-12));
#5192=CARTESIAN_POINT('',(90.0000000000013,283.780735240385,10.0000000000007));
#5193=CARTESIAN_POINT('',(79.1078754759798,283.780735240385,0.));
#5194=CARTESIAN_POINT('',(84.5539377379908,283.780735240385,1.47437617670221E-12));
#5195=CARTESIAN_POINT('',(79.1078754759798,283.780735240385,0.));
#5196=CARTESIAN_POINT('Origin',(79.1078754759798,291.395629230499,0.));
#5197=CARTESIAN_POINT('Origin',(79.1078754759798,291.395629230499,20.0000000000015));
#5198=CARTESIAN_POINT('Origin',(79.1078754759798,291.395629230499,1.47437617670221E-12));
#5199=CARTESIAN_POINT('Origin',(114.902144094842,473.010523220612,0.));
#5200=CARTESIAN_POINT('',(79.1078754759798,473.010523220612,20.0000000000015));
#5201=CARTESIAN_POINT('',(90.0000000000013,473.010523220612,20.0000000000015));
#5202=CARTESIAN_POINT('',(83.2041524529793,473.010523220612,20.0000000000015));
#5203=CARTESIAN_POINT('',(79.1078754759798,473.010523220612,0.));
#5204=CARTESIAN_POINT('',(79.1078754759798,473.010523220612,0.));
#5205=CARTESIAN_POINT('',(90.0000000000013,473.010523220612,1.47437617670221E-12));
#5206=CARTESIAN_POINT('',(102.451072047422,473.010523220612,1.47437617670221E-12));
#5207=CARTESIAN_POINT('',(90.0000000000013,473.010523220612,10.0000000000007));
#5208=CARTESIAN_POINT('Origin',(79.1078754759798,457.780735240385,0.));
#5209=CARTESIAN_POINT('',(90.0000000000013,457.780735240385,20.0000000000015));
#5210=CARTESIAN_POINT('',(79.1078754759798,457.780735240385,20.0000000000015));
#5211=CARTESIAN_POINT('',(65.3070181435484,457.780735240385,20.0000000000015));
#5212=CARTESIAN_POINT('',(90.0000000000013,457.780735240385,1.47437617670221E-12));
#5213=CARTESIAN_POINT('',(90.0000000000013,457.780735240385,10.0000000000007));
#5214=CARTESIAN_POINT('',(79.1078754759798,457.780735240385,0.));
#5215=CARTESIAN_POINT('',(84.553937737991,457.780735240385,1.47437617670221E-12));
#5216=CARTESIAN_POINT('',(79.1078754759798,457.780735240385,0.));
#5217=CARTESIAN_POINT('Origin',(79.1078754759798,465.395629230499,0.));
#5218=CARTESIAN_POINT('Origin',(79.1078754759798,465.395629230499,20.0000000000015));
#5219=CARTESIAN_POINT('Origin',(79.1078754759798,465.395629230499,1.47437617670221E-12));
#5220=CARTESIAN_POINT('Origin',(90.0000000000013,0.,20.0000000000015));
#5221=CARTESIAN_POINT('',(90.0000000000013,505.5,1.47437617670221E-12));
#5222=CARTESIAN_POINT('',(90.0000000000013,0.,1.47437617670221E-12));
#5223=CARTESIAN_POINT('',(90.0000000000013,505.5,20.0000000000015));
#5224=CARTESIAN_POINT('',(90.0000000000013,505.5,1.47437617670221E-12));
#5225=CARTESIAN_POINT('',(90.0000000000013,0.,20.0000000000015));
#5226=CARTESIAN_POINT('Origin',(90.0000000000013,0.,20.0000000000015));
#5227=CARTESIAN_POINT('',(90.0000000000013,0.,1.47437617670221E-12));
#5228=CARTESIAN_POINT('',(90.0000000000013,0.,20.0000000000015));
#5229=CARTESIAN_POINT('Origin',(90.0000000000013,0.,20.0000000000015));
#5230=CARTESIAN_POINT('',(90.0000000000013,37.,20.0000000000015));
#5231=CARTESIAN_POINT('',(90.0000000000013,0.,20.0000000000015));
#5232=CARTESIAN_POINT('',(90.0000000000013,37.,1.47437617670221E-12));
#5233=CARTESIAN_POINT('',(90.0000000000013,37.,36.2500000000015));
#5234=CARTESIAN_POINT('',(90.0000000000013,0.,1.47437617670221E-12));
#5235=CARTESIAN_POINT('Origin',(90.0000000000013,0.,20.0000000000015));
#5236=CARTESIAN_POINT('',(90.0000000000013,0.,1.47437617670221E-12));
#5237=CARTESIAN_POINT('',(90.0000000000013,0.,20.0000000000015));
#5238=CARTESIAN_POINT('Origin',(90.0000000000013,0.,1.47437617670221E-12));
#5239=CARTESIAN_POINT('',(-89.9999999999987,505.5,1.47437617670221E-12));
#5240=CARTESIAN_POINT('',(45.0000000000012,37.,1.47437617670221E-12));
#5241=CARTESIAN_POINT('Origin',(0.,482.5,62.5000000000015));
#5242=CARTESIAN_POINT('',(-31.5061608111161,482.5,105.000000000001));
#5243=CARTESIAN_POINT('',(31.5061608111161,482.5,105.000000000001));
#5244=CARTESIAN_POINT('',(-89.9999999999987,482.5,105.000000000001));
#5245=CARTESIAN_POINT('',(-31.5061608111161,482.5,20.0000000000015));
#5246=CARTESIAN_POINT('',(-31.5061608111161,482.5,83.7500000000015));
#5247=CARTESIAN_POINT('',(31.5061608111161,482.5,20.0000000000015));
#5248=CARTESIAN_POINT('',(-15.7530804055581,482.5,20.0000000000015));
#5249=CARTESIAN_POINT('',(31.5061608111161,482.5,41.2500000000015));
#5250=CARTESIAN_POINT('Origin',(31.5061608111161,0.,20.0000000000015));
#5251=CARTESIAN_POINT('',(31.5061608111161,60.,20.0000000000015));
#5252=CARTESIAN_POINT('',(31.5061608111161,0.,20.0000000000015));
#5253=CARTESIAN_POINT('',(31.5061608111161,60.,105.000000000001));
#5254=CARTESIAN_POINT('',(31.5061608111161,60.,41.2500000000015));
#5255=CARTESIAN_POINT('',(31.5061608111161,0.,105.000000000001));
#5256=CARTESIAN_POINT('Origin',(-31.5061608111161,0.,20.0000000000015));
#5257=CARTESIAN_POINT('',(-31.5061608111161,60.,20.0000000000015));
#5258=CARTESIAN_POINT('',(-31.5061608111161,0.,20.0000000000015));
#5259=CARTESIAN_POINT('',(-15.7530804055581,60.,20.0000000000015));
#5260=CARTESIAN_POINT('Origin',(-31.5061608111161,0.,105.000000000001));
#5261=CARTESIAN_POINT('',(-31.5061608111161,60.,105.000000000001));
#5262=CARTESIAN_POINT('',(-31.5061608111161,0.,105.000000000001));
#5263=CARTESIAN_POINT('',(-31.5061608111161,60.,83.7500000000015));
#5264=CARTESIAN_POINT('Origin',(0.,60.,62.5000000000015));
#5265=CARTESIAN_POINT('',(-89.9999999999987,60.,105.000000000001));
#5266=CARTESIAN_POINT('Origin',(1.24344978758018E-12,37.,52.5000000000015));
#5267=CARTESIAN_POINT('',(-67.5061608111161,37.,105.000000000001));
#5268=CARTESIAN_POINT('',(67.5061608111161,37.,105.000000000001));
#5269=CARTESIAN_POINT('',(15.7530804055587,37.,105.000000000001));
#5270=CARTESIAN_POINT('',(-67.5061608111161,37.,85.0000000000015));
#5271=CARTESIAN_POINT('',(-67.5061608111161,37.,68.7500000000015));
#5272=CARTESIAN_POINT('',(-51.5061608111161,37.,85.0000000000015));
#5273=CARTESIAN_POINT('',(-25.7530804055574,37.,85.0000000000015));
#5274=CARTESIAN_POINT('',(-51.5061608111161,37.,36.2500000000015));
#5275=CARTESIAN_POINT('',(51.5061608111161,37.,20.0000000000015));
#5276=CARTESIAN_POINT('',(25.7530804055587,37.,20.0000000000015));
#5277=CARTESIAN_POINT('',(51.5061608111161,37.,85.0000000000015));
#5278=CARTESIAN_POINT('',(51.5061608111161,37.,68.7500000000015));
#5279=CARTESIAN_POINT('',(67.5061608111161,37.,85.0000000000015));
#5280=CARTESIAN_POINT('',(33.7530804055587,37.,85.0000000000015));
#5281=CARTESIAN_POINT('',(67.5061608111161,37.,78.7500000000015));
#5282=CARTESIAN_POINT('Origin',(-51.5061608111161,0.,20.0000000000015));
#5283=CARTESIAN_POINT('',(-51.5061608111161,505.5,85.0000000000015));
#5284=CARTESIAN_POINT('',(-51.5061608111161,0.,85.0000000000015));
#5285=CARTESIAN_POINT('',(-51.5061608111161,505.5,1.47437617670221E-12));
#5286=CARTESIAN_POINT('Origin',(-51.5061608111161,0.,85.0000000000015));
#5287=CARTESIAN_POINT('',(-67.5061608111161,505.5,85.0000000000015));
#5288=CARTESIAN_POINT('',(-67.5061608111161,0.,85.0000000000015));
#5289=CARTESIAN_POINT('',(-67.5061608111161,505.5,85.0000000000015));
#5290=CARTESIAN_POINT('Origin',(-67.5061608111161,0.,85.0000000000015));
#5291=CARTESIAN_POINT('',(-67.5061608111161,505.5,105.000000000001));
#5292=CARTESIAN_POINT('',(-67.5061608111161,0.,105.000000000001));
#5293=CARTESIAN_POINT('',(-67.5061608111161,505.5,105.000000000001));
#5294=CARTESIAN_POINT('Origin',(31.5061608111161,0.,105.000000000001));
#5295=CARTESIAN_POINT('',(67.5061608111161,505.5,105.000000000001));
#5296=CARTESIAN_POINT('',(-51.5061608111161,505.5,105.000000000001));
#5297=CARTESIAN_POINT('',(67.5061608111161,0.,105.000000000001));
#5298=CARTESIAN_POINT('Origin',(51.5061608111161,0.,20.0000000000015));
#5299=CARTESIAN_POINT('',(51.5061608111161,505.5,20.0000000000015));
#5300=CARTESIAN_POINT('',(90.0000000000013,505.5,20.0000000000015));
#5301=CARTESIAN_POINT('',(51.5061608111161,0.,20.0000000000015));
#5302=CARTESIAN_POINT('Origin',(51.5061608111161,0.,85.0000000000015));
#5303=CARTESIAN_POINT('',(51.5061608111161,505.5,85.0000000000015));
#5304=CARTESIAN_POINT('',(51.5061608111161,505.5,1.47437617670221E-12));
#5305=CARTESIAN_POINT('',(51.5061608111161,0.,85.0000000000015));
#5306=CARTESIAN_POINT('Origin',(67.5061608111161,0.,85.0000000000015));
#5307=CARTESIAN_POINT('',(67.5061608111161,505.5,85.0000000000015));
#5308=CARTESIAN_POINT('',(67.5061608111161,505.5,85.0000000000015));
#5309=CARTESIAN_POINT('',(67.5061608111161,0.,85.0000000000015));
#5310=CARTESIAN_POINT('Origin',(67.5061608111161,0.,105.000000000001));
#5311=CARTESIAN_POINT('',(67.5061608111161,505.5,105.000000000001));
#5312=CARTESIAN_POINT('Origin',(1.24344978758018E-12,505.5,52.5000000000015));
#5313=CARTESIAN_POINT('',(0.,0.,0.));
#5314=CARTESIAN_POINT('Origin',(4.44089209850063E-15,581.925982185852,41.5000000000007));
#5315=CARTESIAN_POINT('',(2.9713159395238E-15,582.425982185852,29.5000000000007));
#5316=CARTESIAN_POINT('Origin',(4.44089209850063E-15,582.425982185852,41.5000000000007));
#5317=CARTESIAN_POINT('',(2.91008359956643E-15,581.925982185852,29.0000000000007));
#5318=CARTESIAN_POINT('Origin',(2.9713159395238E-15,581.925982185852,29.5000000000007));
#5319=CARTESIAN_POINT('',(12.5,581.925982185852,41.5000000000007));
#5320=CARTESIAN_POINT('Origin',(4.44089209850063E-15,581.925982185852,41.5000000000007));
#5321=CARTESIAN_POINT('Origin',(4.44089209850063E-15,581.925982185852,41.5000000000007));
#5322=CARTESIAN_POINT('Origin',(4.44089209850063E-15,552.425982185852,41.5000000000007));
#5323=CARTESIAN_POINT('',(12.5,552.925982185852,41.5000000000007));
#5324=CARTESIAN_POINT('',(12.5,552.425982185852,41.5000000000007));
#5325=CARTESIAN_POINT('',(2.91008359956643E-15,552.925982185852,29.0000000000007));
#5326=CARTESIAN_POINT('Origin',(4.44089209850063E-15,552.925982185852,41.5000000000007));
#5327=CARTESIAN_POINT('Origin',(4.44089209850063E-15,552.925982185852,41.5000000000007));
#5328=CARTESIAN_POINT('Origin',(4.44089209850063E-15,582.425982185852,41.5000000000007));
#5329=CARTESIAN_POINT('',(7.5,582.425982185852,41.5000000000007));
#5330=CARTESIAN_POINT('Origin',(4.44089209850063E-15,582.425982185852,41.5000000000007));
#5331=CARTESIAN_POINT('Origin',(4.44089209850063E-15,552.925982185852,41.5000000000007));
#5332=CARTESIAN_POINT('',(2.9713159395238E-15,552.425982185852,29.5000000000007));
#5333=CARTESIAN_POINT('Origin',(2.9713159395238E-15,552.925982185852,29.5000000000007));
#5334=CARTESIAN_POINT('Origin',(4.44089209850063E-15,552.425982185852,41.5000000000007));
#5335=CARTESIAN_POINT('Origin',(4.44089209850063E-15,552.425982185852,41.5000000000007));
#5336=CARTESIAN_POINT('',(7.5,552.425982185852,41.5000000000007));
#5337=CARTESIAN_POINT('Origin',(4.44089209850063E-15,552.425982185852,41.5000000000007));
#5338=CARTESIAN_POINT('Origin',(4.44089209850063E-15,552.425982185852,41.5000000000007));
#5339=CARTESIAN_POINT('',(7.5,552.425982185852,41.5000000000007));
#5340=CARTESIAN_POINT('',(0.,0.,0.));
#5341=CARTESIAN_POINT('Origin',(4.44089209850063E-15,36.9999821858522,41.5000000000007));
#5342=CARTESIAN_POINT('',(-11.5112,343.,41.5000000000007));
#5343=CARTESIAN_POINT('Origin',(4.44089209850063E-15,343.,41.5000000000007));
#5344=CARTESIAN_POINT('',(-11.5112,363.,41.5000000000007));
#5345=CARTESIAN_POINT('',(-11.5112,36.9999821858522,41.5000000000007));
#5346=CARTESIAN_POINT('Origin',(4.44089209850063E-15,363.,41.5000000000007));
#5347=CARTESIAN_POINT('Origin',(-31.5061608111161,363.,85.0000000000015));
#5348=CARTESIAN_POINT('',(31.5058391888839,363.,85.0000000000015));
#5349=CARTESIAN_POINT('',(-31.5061608111161,363.,85.0000000000015));
#5350=CARTESIAN_POINT('',(-0.000160811116123316,363.,85.0000000000015));
#5351=CARTESIAN_POINT('',(31.5058391888839,363.,25.0000000000015));
#5352=CARTESIAN_POINT('',(31.5058391888839,363.,85.0000000000015));
#5353=CARTESIAN_POINT('',(-31.5061608111161,363.,25.0000000000015));
#5354=CARTESIAN_POINT('',(31.5058391888839,363.,25.0000000000015));
#5355=CARTESIAN_POINT('',(-31.5061608111161,363.,85.0000000000015));
#5356=CARTESIAN_POINT('Origin',(31.5058391888839,343.,85.0000000000015));
#5357=CARTESIAN_POINT('',(-31.5061608111161,343.,85.0000000000015));
#5358=CARTESIAN_POINT('',(31.5058391888839,343.,85.0000000000015));
#5359=CARTESIAN_POINT('',(31.5058391888839,343.,85.0000000000015));
#5360=CARTESIAN_POINT('',(-31.5061608111161,343.,25.0000000000015));
#5361=CARTESIAN_POINT('',(-31.5061608111161,343.,85.0000000000015));
#5362=CARTESIAN_POINT('',(31.5058391888839,343.,25.0000000000015));
#5363=CARTESIAN_POINT('',(-31.5061608111161,343.,25.0000000000015));
#5364=CARTESIAN_POINT('',(31.5058391888839,343.,85.0000000000015));
#5365=CARTESIAN_POINT('Origin',(-0.000160811116125537,353.,25.0000000000015));
#5366=CARTESIAN_POINT('',(-31.5061608111161,363.,25.0000000000015));
#5367=CARTESIAN_POINT('',(31.5058391888839,343.,25.0000000000015));
#5368=CARTESIAN_POINT('Origin',(31.5058391888839,245.5,85.0000000000015));
#5369=CARTESIAN_POINT('',(-31.5061608111161,460.5,85.0000000000015));
#5370=CARTESIAN_POINT('',(-31.5061608111161,245.5,85.0000000000015));
#5371=CARTESIAN_POINT('',(31.5058391888839,460.5,85.0000000000015));
#5372=CARTESIAN_POINT('',(31.5058391888839,460.5,85.0000000000015));
#5373=CARTESIAN_POINT('',(31.5058391888839,245.5,85.0000000000015));
#5374=CARTESIAN_POINT('Origin',(31.5058391888839,245.5,85.0000000000015));
#5375=CARTESIAN_POINT('',(31.5058391888839,245.5,85.0000000000015));
#5376=CARTESIAN_POINT('',(31.5058391888839,245.5,85.0000000000015));
#5377=CARTESIAN_POINT('',(-31.5061608111161,245.5,85.0000000000015));
#5378=CARTESIAN_POINT('',(31.5058391888839,245.5,85.0000000000015));
#5379=CARTESIAN_POINT('',(-31.5061608111161,245.5,85.0000000000015));
#5380=CARTESIAN_POINT('Origin',(-31.5061608111161,245.5,105.000000000001));
#5381=CARTESIAN_POINT('',(31.5058391888839,336.294725687261,105.000000000001));
#5382=CARTESIAN_POINT('',(31.5058391888839,330.773057370623,105.000000000001));
#5383=CARTESIAN_POINT('Origin',(21.8945024061954,333.533891528942,105.000000000001));
#5384=CARTESIAN_POINT('',(31.5058391888839,245.5,105.000000000001));
#5385=CARTESIAN_POINT('Origin',(-31.5061608111161,245.5,105.000000000001));
#5386=CARTESIAN_POINT('',(-31.5061608111161,330.774177285199,105.000000000001));
#5387=CARTESIAN_POINT('',(-11.8945024061954,333.533891528942,105.000000000001));
#5388=CARTESIAN_POINT('Origin',(-21.8945024061954,333.533891528942,105.000000000001));
#5389=CARTESIAN_POINT('',(-31.5061608111161,336.293605772685,105.000000000001));
#5390=CARTESIAN_POINT('Origin',(-21.8945024061954,333.533891528942,105.000000000001));
#5391=CARTESIAN_POINT('',(-31.5061608111161,245.5,105.000000000001));
#5392=CARTESIAN_POINT('Origin',(-31.5061608111161,245.5,105.000000000001));
#5393=CARTESIAN_POINT('',(-31.5061608111161,370.774177285199,105.000000000001));
#5394=CARTESIAN_POINT('',(-11.8945024061954,373.533891528942,105.000000000001));
#5395=CARTESIAN_POINT('Origin',(-21.8945024061954,373.533891528942,105.000000000001));
#5396=CARTESIAN_POINT('',(-31.5061608111161,376.293605772685,105.000000000001));
#5397=CARTESIAN_POINT('Origin',(-21.8945024061954,373.533891528942,105.000000000001));
#5398=CARTESIAN_POINT('',(-31.5061608111161,245.5,105.000000000001));
#5399=CARTESIAN_POINT('Origin',(-31.5061608111161,245.5,105.000000000001));
#5400=CARTESIAN_POINT('',(31.5058391888839,376.294725687261,105.000000000001));
#5401=CARTESIAN_POINT('',(31.5058391888839,370.773057370623,105.000000000001));
#5402=CARTESIAN_POINT('Origin',(21.8945024061954,373.533891528942,105.000000000001));
#5403=CARTESIAN_POINT('',(31.5058391888839,245.5,105.000000000001));
#5404=CARTESIAN_POINT('Origin',(31.5058391888839,245.5,105.000000000001));
#5405=CARTESIAN_POINT('',(31.5058391888839,245.5,105.000000000001));
#5406=CARTESIAN_POINT('',(31.5058391888839,245.5,105.000000000001));
#5407=CARTESIAN_POINT('',(31.5058391888839,460.5,105.000000000001));
#5408=CARTESIAN_POINT('',(31.5058391888839,460.5,105.000000000001));
#5409=CARTESIAN_POINT('',(31.5058391888839,365.5,105.000000000001));
#5410=CARTESIAN_POINT('',(31.5058391888839,365.5,105.000000000001));
#5411=CARTESIAN_POINT('',(31.5058391888839,365.5,105.000000000001));
#5412=CARTESIAN_POINT('Origin',(-31.5061608111161,245.5,85.0000000000015));
#5413=CARTESIAN_POINT('',(-31.5061608111161,245.5,105.000000000001));
#5414=CARTESIAN_POINT('',(-31.5061608111161,245.5,85.0000000000015));
#5415=CARTESIAN_POINT('',(-31.5061608111161,365.5,105.000000000001));
#5416=CARTESIAN_POINT('',(-31.5061608111161,365.5,105.000000000001));
#5417=CARTESIAN_POINT('',(-31.5061608111161,460.5,105.000000000001));
#5418=CARTESIAN_POINT('',(-31.5061608111161,365.5,105.000000000001));
#5419=CARTESIAN_POINT('',(-31.5061608111161,460.5,85.0000000000015));
#5420=CARTESIAN_POINT('Origin',(0.,485.5,105.000000000001));
#5421=CARTESIAN_POINT('Origin',(-21.8945024061954,373.533891528942,105.000000000001));
#5422=CARTESIAN_POINT('Origin',(-21.8945024061954,333.533891528942,105.000000000001));
#5423=CARTESIAN_POINT('',(-67.5061608111161,245.5,105.000000000001));
#5424=CARTESIAN_POINT('',(67.5061608111161,245.5,105.000000000001));
#5425=CARTESIAN_POINT('',(-67.5061608111161,460.5,105.000000000001));
#5426=CARTESIAN_POINT('',(-67.5061608111161,485.5,105.000000000001));
#5427=CARTESIAN_POINT('',(20.626540202779,460.5,105.000000000001));
#5428=CARTESIAN_POINT('Origin',(0.,485.5,105.000000000001));
#5429=CARTESIAN_POINT('',(67.5061608111161,460.5,105.000000000001));
#5430=CARTESIAN_POINT('',(20.626540202779,460.5,105.000000000001));
#5431=CARTESIAN_POINT('',(67.5061608111161,245.5,105.000000000001));
#5432=CARTESIAN_POINT('',(67.5061608111161,485.5,105.000000000001));
#5433=CARTESIAN_POINT('',(67.5061608111161,245.5,105.000000000001));
#5434=CARTESIAN_POINT('',(31.8945024061955,333.533891528942,105.000000000001));
#5435=CARTESIAN_POINT('Origin',(21.8945024061954,333.533891528942,105.000000000001));
#5436=CARTESIAN_POINT('Origin',(21.8945024061954,333.533891528942,105.000000000001));
#5437=CARTESIAN_POINT('',(31.8945024061955,373.533891528942,105.000000000001));
#5438=CARTESIAN_POINT('Origin',(21.8945024061954,373.533891528942,105.000000000001));
#5439=CARTESIAN_POINT('Origin',(21.8945024061954,373.533891528942,105.000000000001));
#5440=CARTESIAN_POINT('Origin',(-21.8945024061954,373.533891528942,120.000000000001));
#5441=CARTESIAN_POINT('',(-11.8945024061954,373.533891528942,120.000000000001));
#5442=CARTESIAN_POINT('Origin',(-21.8945024061954,373.533891528942,120.000000000001));
#5443=CARTESIAN_POINT('',(-11.8945024061954,373.533891528942,120.000000000001));
#5444=CARTESIAN_POINT('Origin',(21.8945024061954,373.533891528942,120.000000000001));
#5445=CARTESIAN_POINT('',(31.8945024061955,373.533891528942,120.000000000001));
#5446=CARTESIAN_POINT('Origin',(21.8945024061954,373.533891528942,120.000000000001));
#5447=CARTESIAN_POINT('',(31.8945024061955,373.533891528942,120.000000000001));
#5448=CARTESIAN_POINT('Origin',(-21.8945024061954,333.533891528942,120.000000000001));
#5449=CARTESIAN_POINT('',(-11.8945024061954,333.533891528942,120.000000000001));
#5450=CARTESIAN_POINT('Origin',(-21.8945024061954,333.533891528942,120.000000000001));
#5451=CARTESIAN_POINT('',(-11.8945024061954,333.533891528942,120.000000000001));
#5452=CARTESIAN_POINT('Origin',(21.8945024061954,333.533891528942,120.000000000001));
#5453=CARTESIAN_POINT('',(31.8945024061955,333.533891528942,120.000000000001));
#5454=CARTESIAN_POINT('Origin',(21.8945024061954,333.533891528942,120.000000000001));
#5455=CARTESIAN_POINT('',(31.8945024061955,333.533891528942,120.000000000001));
#5456=CARTESIAN_POINT('Origin',(-67.5061608111161,485.5,105.000000000001));
#5457=CARTESIAN_POINT('',(-67.5061608111161,460.5,85.0000000000015));
#5458=CARTESIAN_POINT('',(-67.5061608111161,460.5,98.7500000000015));
#5459=CARTESIAN_POINT('',(-67.5061608111161,245.5,85.0000000000015));
#5460=CARTESIAN_POINT('',(-67.5061608111161,245.5,105.000000000001));
#5461=CARTESIAN_POINT('',(-67.5061608111161,485.5,85.0000000000015));
#5462=CARTESIAN_POINT('Origin',(-67.5061608111161,485.5,85.0000000000015));
#5463=CARTESIAN_POINT('',(-51.5061608111161,460.5,85.0000000000015));
#5464=CARTESIAN_POINT('',(-54.3796206083371,460.5,85.0000000000015));
#5465=CARTESIAN_POINT('',(-51.5061608111161,245.5,85.0000000000015));
#5466=CARTESIAN_POINT('',(-67.5061608111161,245.5,85.0000000000015));
#5467=CARTESIAN_POINT('',(-51.5061608111161,485.5,85.0000000000015));
#5468=CARTESIAN_POINT('Origin',(-51.5061608111161,485.5,85.0000000000015));
#5469=CARTESIAN_POINT('',(-51.5061608111161,460.5,65.0000000000015));
#5470=CARTESIAN_POINT('',(-51.5061608111161,460.5,88.7500000000015));
#5471=CARTESIAN_POINT('',(-51.5061608111161,245.5,65.0000000000015));
#5472=CARTESIAN_POINT('',(-51.5061608111161,245.5,85.0000000000015));
#5473=CARTESIAN_POINT('',(-51.5061608111161,485.5,65.0000000000015));
#5474=CARTESIAN_POINT('Origin',(-82.5061608111161,485.5,65.0000000000015));
#5475=CARTESIAN_POINT('',(-82.5061608111161,460.5,65.0000000000015));
#5476=CARTESIAN_POINT('',(-82.5061608111161,460.5,120.000000000001));
#5477=CARTESIAN_POINT('',(-82.5061608111161,460.5,78.7500000000015));
#5478=CARTESIAN_POINT('',(-82.5061608111161,245.5,65.0000000000015));
#5479=CARTESIAN_POINT('',(-82.5061608111161,485.5,65.0000000000015));
#5480=CARTESIAN_POINT('',(-82.5061608111161,245.5,120.000000000001));
#5481=CARTESIAN_POINT('',(-82.5061608111161,245.5,20.0000000000015));
#5482=CARTESIAN_POINT('',(-82.5061608111161,485.5,120.000000000001));
#5483=CARTESIAN_POINT('Origin',(-51.5061608111161,485.5,65.0000000000015));
#5484=CARTESIAN_POINT('',(-46.3796206083371,460.5,65.0000000000015));
#5485=CARTESIAN_POINT('',(-51.5061608111161,245.5,65.0000000000015));
#5486=CARTESIAN_POINT('Origin',(41.2530804055581,460.5,92.5000000000015));
#5487=CARTESIAN_POINT('',(51.5061608111161,460.5,85.0000000000015));
#5488=CARTESIAN_POINT('',(51.5061608111161,460.5,65.0000000000015));
#5489=CARTESIAN_POINT('',(51.5061608111161,460.5,88.7500000000015));
#5490=CARTESIAN_POINT('',(67.5061608111161,460.5,85.0000000000015));
#5491=CARTESIAN_POINT('',(54.3796206083371,460.5,85.0000000000015));
#5492=CARTESIAN_POINT('',(67.5061608111161,460.5,98.7500000000015));
#5493=CARTESIAN_POINT('',(82.5061608111161,460.5,120.000000000001));
#5494=CARTESIAN_POINT('',(-61.8796206083371,460.5,120.000000000001));
#5495=CARTESIAN_POINT('',(82.5061608111161,460.5,65.0000000000015));
#5496=CARTESIAN_POINT('',(82.5061608111161,460.5,78.7500000000015));
#5497=CARTESIAN_POINT('',(46.3796206083371,460.5,65.0000000000015));
#5498=CARTESIAN_POINT('Origin',(67.5061608111161,485.5,105.000000000001));
#5499=CARTESIAN_POINT('',(67.5061608111161,245.5,85.0000000000015));
#5500=CARTESIAN_POINT('',(67.5061608111161,485.5,85.0000000000015));
#5501=CARTESIAN_POINT('',(67.5061608111161,245.5,105.000000000001));
#5502=CARTESIAN_POINT('Origin',(67.5061608111161,485.5,85.0000000000015));
#5503=CARTESIAN_POINT('',(51.5061608111161,245.5,85.0000000000015));
#5504=CARTESIAN_POINT('',(51.5061608111161,485.5,85.0000000000015));
#5505=CARTESIAN_POINT('',(67.5061608111161,245.5,85.0000000000015));
#5506=CARTESIAN_POINT('Origin',(51.5061608111161,485.5,85.0000000000015));
#5507=CARTESIAN_POINT('',(51.5061608111161,245.5,65.0000000000015));
#5508=CARTESIAN_POINT('',(51.5061608111161,485.5,65.0000000000015));
#5509=CARTESIAN_POINT('',(51.5061608111161,245.5,85.0000000000015));
#5510=CARTESIAN_POINT('Origin',(82.5061608111161,485.5,120.000000000001));
#5511=CARTESIAN_POINT('',(82.5061608111161,245.5,120.000000000001));
#5512=CARTESIAN_POINT('',(82.5061608111161,245.5,120.000000000001));
#5513=CARTESIAN_POINT('',(82.5061608111161,485.5,120.000000000001));
#5514=CARTESIAN_POINT('Origin',(82.5061608111161,485.5,65.0000000000015));
#5515=CARTESIAN_POINT('',(82.5061608111161,245.5,65.0000000000015));
#5516=CARTESIAN_POINT('',(82.5061608111161,245.5,20.0000000000015));
#5517=CARTESIAN_POINT('',(82.5061608111161,485.5,65.0000000000015));
#5518=CARTESIAN_POINT('Origin',(51.5061608111161,485.5,65.0000000000015));
#5519=CARTESIAN_POINT('',(51.5061608111161,245.5,65.0000000000015));
#5520=CARTESIAN_POINT('Origin',(41.2530804055581,245.5,92.5000000000015));
#5521=CARTESIAN_POINT('',(0.,0.,0.));
#5522=CARTESIAN_POINT('Origin',(-25.,600.5,16.5000000000007));
#5523=CARTESIAN_POINT('',(-30.,730.5,16.5000000000007));
#5524=CARTESIAN_POINT('',(-25.,730.5,11.5000000000007));
#5525=CARTESIAN_POINT('Origin',(-25.,730.5,16.5000000000007));
#5526=CARTESIAN_POINT('',(-25.,600.5,11.5000000000007));
#5527=CARTESIAN_POINT('',(-25.,600.5,11.5000000000007));
#5528=CARTESIAN_POINT('',(-30.,600.5,16.5000000000007));
#5529=CARTESIAN_POINT('Origin',(-25.,600.5,16.5000000000007));
#5530=CARTESIAN_POINT('',(-30.,600.5,16.5000000000007));
#5531=CARTESIAN_POINT('Origin',(0.,600.5,41.5000000000007));
#5532=CARTESIAN_POINT('',(25.,600.5,11.5000000000007));
#5533=CARTESIAN_POINT('',(30.,600.5,11.5000000000007));
#5534=CARTESIAN_POINT('',(30.,600.5,16.5000000000007));
#5535=CARTESIAN_POINT('Origin',(25.,600.5,16.5000000000007));
#5536=CARTESIAN_POINT('',(30.,600.5,66.5000000000007));
#5537=CARTESIAN_POINT('',(30.,600.5,71.5000000000007));
#5538=CARTESIAN_POINT('',(25.,600.5,71.5000000000007));
#5539=CARTESIAN_POINT('Origin',(25.,600.5,66.5000000000007));
#5540=CARTESIAN_POINT('',(-25.,600.5,71.5000000000007));
#5541=CARTESIAN_POINT('',(-30.,600.5,71.5000000000007));
#5542=CARTESIAN_POINT('',(-30.,600.5,66.5000000000007));
#5543=CARTESIAN_POINT('Origin',(-25.,600.5,66.5000000000007));
#5544=CARTESIAN_POINT('',(-30.,600.5,11.5000000000007));
#5545=CARTESIAN_POINT('Origin',(30.,600.5,11.5000000000007));
#5546=CARTESIAN_POINT('',(25.,730.5,11.5000000000007));
#5547=CARTESIAN_POINT('',(30.,730.5,11.5000000000007));
#5548=CARTESIAN_POINT('',(25.,600.5,11.5000000000007));
#5549=CARTESIAN_POINT('Origin',(25.,600.5,16.5000000000007));
#5550=CARTESIAN_POINT('',(30.,730.5,16.5000000000007));
#5551=CARTESIAN_POINT('Origin',(25.,730.5,16.5000000000007));
#5552=CARTESIAN_POINT('',(30.,600.5,16.5000000000007));
#5553=CARTESIAN_POINT('Origin',(-25.,600.5,66.5000000000007));
#5554=CARTESIAN_POINT('',(-25.,730.5,71.5000000000007));
#5555=CARTESIAN_POINT('',(-30.,730.5,66.5000000000007));
#5556=CARTESIAN_POINT('Origin',(-25.,730.5,66.5000000000007));
#5557=CARTESIAN_POINT('',(-30.,600.5,66.5000000000007));
#5558=CARTESIAN_POINT('',(-25.,600.5,71.5000000000007));
#5559=CARTESIAN_POINT('Origin',(-30.,600.5,71.5000000000007));
#5560=CARTESIAN_POINT('',(25.,730.5,71.5000000000007));
#5561=CARTESIAN_POINT('',(25.,600.5,71.5000000000007));
#5562=CARTESIAN_POINT('',(-30.,730.5,71.5000000000007));
#5563=CARTESIAN_POINT('Origin',(25.,600.5,66.5000000000007));
#5564=CARTESIAN_POINT('',(30.,730.5,66.5000000000007));
#5565=CARTESIAN_POINT('Origin',(25.,730.5,66.5000000000007));
#5566=CARTESIAN_POINT('',(30.,600.5,66.5000000000007));
#5567=CARTESIAN_POINT('Origin',(30.,600.5,71.5000000000007));
#5568=CARTESIAN_POINT('',(30.,730.5,71.5000000000007));
#5569=CARTESIAN_POINT('Origin',(-30.,600.5,11.5000000000007));
#5570=CARTESIAN_POINT('',(-30.,730.5,11.5000000000007));
#5571=CARTESIAN_POINT('Origin',(0.,730.5,41.5000000000007));
#5572=CARTESIAN_POINT('',(0.,0.,0.));
#5573=CARTESIAN_POINT('Origin',(4.44089209850063E-15,525.425982185852,41.5000000000007));
#5574=CARTESIAN_POINT('',(7.50000000000001,585.425982185852,41.5000000000007));
#5575=CARTESIAN_POINT('Origin',(4.44089209850063E-15,585.425982185852,41.5000000000007));
#5576=CARTESIAN_POINT('',(7.50000000000001,525.425982185852,41.5000000000007));
#5577=CARTESIAN_POINT('',(7.50000000000001,525.425982185852,41.5000000000007));
#5578=CARTESIAN_POINT('Origin',(4.44089209850063E-15,525.425982185852,41.5000000000007));
#5579=CARTESIAN_POINT('Origin',(4.44089209850063E-15,585.425982185852,41.5000000000007));
#5580=CARTESIAN_POINT('Origin',(4.44089209850063E-15,525.425982185852,41.5000000000007));
#5581=CARTESIAN_POINT('',(10.88225,36.9999821858522,41.5000000000007));
#5582=CARTESIAN_POINT('Origin',(4.44089209850063E-15,36.9999821858522,41.5000000000007));
#5583=CARTESIAN_POINT('',(10.88225,525.425982185852,41.5000000000007));
#5584=CARTESIAN_POINT('',(10.88225,525.425982185852,41.5000000000007));
#5585=CARTESIAN_POINT('Origin',(4.44089209850063E-15,525.425982185852,41.5000000000007));
#5586=CARTESIAN_POINT('Origin',(4.44089209850063E-15,525.425982185852,41.5000000000007));
#5587=CARTESIAN_POINT('Origin',(4.44089209850063E-15,36.9999821858522,41.5000000000007));
#5588=CARTESIAN_POINT('',(0.,0.,0.));
#5589=CARTESIAN_POINT('Origin',(4.44089209850063E-15,525.425982185852,41.5000000000007));
#5590=CARTESIAN_POINT('',(11.,525.425982185852,41.5000000000007));
#5591=CARTESIAN_POINT('Origin',(4.44089209850063E-15,525.425982185852,41.5000000000007));
#5592=CARTESIAN_POINT('',(11.,505.5,41.5000000000007));
#5593=CARTESIAN_POINT('',(11.,525.425982185852,41.5000000000007));
#5594=CARTESIAN_POINT('Origin',(4.44089209850063E-15,505.5,41.5000000000007));
#5595=CARTESIAN_POINT('Origin',(-37.5,585.425982185852,83.));
#5596=CARTESIAN_POINT('',(-37.5,585.425982185852,83.));
#5597=CARTESIAN_POINT('',(37.5,585.425982185852,83.));
#5598=CARTESIAN_POINT('',(-44.5030804055581,585.425982185852,83.));
#5599=CARTESIAN_POINT('',(-37.5,585.425982185852,0.));
#5600=CARTESIAN_POINT('',(-37.5,585.425982185852,83.));
#5601=CARTESIAN_POINT('',(37.5,585.425982185852,0.));
#5602=CARTESIAN_POINT('',(7.00308040555807,585.425982185852,1.47437617670221E-12));
#5603=CARTESIAN_POINT('',(37.5,585.425982185852,83.));
#5604=CARTESIAN_POINT('Origin',(-37.5,525.425982185852,83.));
#5605=CARTESIAN_POINT('',(-37.5,525.425982185852,83.));
#5606=CARTESIAN_POINT('',(-37.5,515.462991092926,83.));
#5607=CARTESIAN_POINT('',(-37.5,525.425982185852,0.));
#5608=CARTESIAN_POINT('',(-37.5,525.425982185852,83.));
#5609=CARTESIAN_POINT('',(-37.5,515.462991092926,1.47437617670221E-12));
#5610=CARTESIAN_POINT('Origin',(37.5,525.425982185852,83.));
#5611=CARTESIAN_POINT('',(37.5,525.425982185852,83.));
#5612=CARTESIAN_POINT('',(-7.00308040555806,525.425982185852,83.));
#5613=CARTESIAN_POINT('',(37.5,525.425982185852,0.));
#5614=CARTESIAN_POINT('',(37.5,525.425982185852,83.));
#5615=CARTESIAN_POINT('',(44.5030804055581,525.425982185852,1.47437617670221E-12));
#5616=CARTESIAN_POINT('Origin',(37.5,585.425982185852,83.));
#5617=CARTESIAN_POINT('',(37.5,545.462991092926,83.));
#5618=CARTESIAN_POINT('',(37.5,545.462991092926,1.47437617670221E-12));
#5619=CARTESIAN_POINT('Origin',(49.0061608111161,505.5,2.50000000000147));
#5620=CARTESIAN_POINT('',(46.5061608111161,600.5,1.47437617670221E-12));
#5621=CARTESIAN_POINT('',(51.5061608111161,600.5,5.00000000000147));
#5622=CARTESIAN_POINT('',(46.5046206083369,600.5,-0.00154020277773892));
#5623=CARTESIAN_POINT('',(51.5061608111161,505.5,5.00000000000147));
#5624=CARTESIAN_POINT('',(51.5061608111161,505.5,5.00000000000147));
#5625=CARTESIAN_POINT('',(46.5061608111161,505.5,1.47437617670221E-12));
#5626=CARTESIAN_POINT('',(46.5046206083369,505.5,-0.00154020277773892));
#5627=CARTESIAN_POINT('',(46.5061608111161,505.5,1.47437617670221E-12));
#5628=CARTESIAN_POINT('Origin',(51.5061608111161,505.5,1.47437617670221E-12));
#5629=CARTESIAN_POINT('',(-46.5061608111161,505.5,1.47437617670221E-12));
#5630=CARTESIAN_POINT('',(90.0000000000013,505.5,1.47437617670221E-12));
#5631=CARTESIAN_POINT('',(-46.5061608111161,600.5,1.47437617670221E-12));
#5632=CARTESIAN_POINT('',(-46.5061608111161,505.5,1.47437617670221E-12));
#5633=CARTESIAN_POINT('',(90.0000000000013,600.5,1.47437617670221E-12));
#5634=CARTESIAN_POINT('Origin',(0.,505.5,41.5000000000007));
#5635=CARTESIAN_POINT('',(51.5061608111161,505.5,78.));
#5636=CARTESIAN_POINT('',(51.5061608111161,505.5,-83.));
#5637=CARTESIAN_POINT('',(46.5061608111161,505.5,83.));
#5638=CARTESIAN_POINT('',(46.5046206083369,505.5,83.0015402027792));
#5639=CARTESIAN_POINT('',(-46.5061608111161,505.5,83.));
#5640=CARTESIAN_POINT('',(51.5061608111161,505.5,83.));
#5641=CARTESIAN_POINT('',(-51.5061608111161,505.5,78.));
#5642=CARTESIAN_POINT('',(-46.5046206083369,505.5,83.0015402027792));
#5643=CARTESIAN_POINT('',(-51.5061608111161,505.5,5.00000000000147));
#5644=CARTESIAN_POINT('',(-51.5061608111161,505.5,83.));
#5645=CARTESIAN_POINT('',(-46.5046206083369,505.5,-0.00154020277773892));
#5646=CARTESIAN_POINT('Origin',(49.0061608111161,505.5,80.5));
#5647=CARTESIAN_POINT('',(51.5061608111161,600.5,78.));
#5648=CARTESIAN_POINT('',(46.5061608111161,600.5,83.));
#5649=CARTESIAN_POINT('',(46.5046206083369,600.5,83.0015402027792));
#5650=CARTESIAN_POINT('',(46.5061608111161,505.5,83.));
#5651=CARTESIAN_POINT('',(51.5061608111161,505.5,78.));
#5652=CARTESIAN_POINT('Origin',(-51.5061608111161,505.5,83.));
#5653=CARTESIAN_POINT('',(-46.5061608111161,600.5,83.));
#5654=CARTESIAN_POINT('',(51.5061608111161,600.5,83.));
#5655=CARTESIAN_POINT('',(-46.5061608111161,505.5,83.));
#5656=CARTESIAN_POINT('Origin',(-49.0061608111161,505.5,80.5));
#5657=CARTESIAN_POINT('',(-51.5061608111161,600.5,78.));
#5658=CARTESIAN_POINT('',(-46.5046206083369,600.5,83.0015402027792));
#5659=CARTESIAN_POINT('',(-51.5061608111161,505.5,78.));
#5660=CARTESIAN_POINT('Origin',(-49.0061608111161,505.5,2.50000000000147));
#5661=CARTESIAN_POINT('',(-51.5061608111161,600.5,5.00000000000147));
#5662=CARTESIAN_POINT('',(-46.5046206083369,600.5,-0.00154020277773892));
#5663=CARTESIAN_POINT('',(-51.5061608111161,505.5,5.00000000000147));
#5664=CARTESIAN_POINT('Origin',(-51.5061608111161,505.5,1.47437617670221E-12));
#5665=CARTESIAN_POINT('',(-51.5061608111161,600.5,83.));
#5666=CARTESIAN_POINT('Origin',(51.5061608111161,505.5,83.));
#5667=CARTESIAN_POINT('',(51.5061608111161,600.5,-83.));
#5668=CARTESIAN_POINT('Origin',(0.,600.5,41.5000000000007));
#5669=CARTESIAN_POINT('',(0.,0.,0.));
#5670=CARTESIAN_POINT('Origin',(4.44089209850063E-15,22.3469309188597,41.5000000000007));
#5671=CARTESIAN_POINT('',(2.96944523434646E-16,24.3469309188597,75.3378998577488));
#5672=CARTESIAN_POINT('Origin',(4.44089209850063E-15,24.3469309188597,41.5000000000007));
#5673=CARTESIAN_POINT('',(5.41873883264117E-16,22.3469309188597,73.3378998577488));
#5674=CARTESIAN_POINT('Origin',(2.96944523434646E-16,22.3469309188597,75.3378998577488));
#5675=CARTESIAN_POINT('Origin',(4.44089209850063E-15,22.3469309188597,41.5000000000007));
#5676=CARTESIAN_POINT('Origin',(4.44089209850063E-15,19.2969601946621,41.5000000000007));
#5677=CARTESIAN_POINT('',(5.41873883264117E-16,16.2469894704645,73.3378998577488));
#5678=CARTESIAN_POINT('Origin',(4.44089209850063E-15,16.2469894704645,41.5000000000007));
#5679=CARTESIAN_POINT('',(5.41873883264117E-16,19.2969601946621,73.3378998577488));
#5680=CARTESIAN_POINT('Origin',(4.44089209850063E-15,24.3469309188597,9.66210014225272));
#5681=CARTESIAN_POINT('',(1.68360194775942E-16,24.3469309188597,76.3878705819464));
#5682=CARTESIAN_POINT('Origin',(4.44089209850063E-15,24.3469309188597,41.5000000000007));
#5683=CARTESIAN_POINT('Origin',(4.44089209850063E-15,12.2469894704645,41.5000000000007));
#5684=CARTESIAN_POINT('',(2.48799989461716E-15,14.2469894704645,57.4465750063058));
#5685=CARTESIAN_POINT('Origin',(4.44089209850063E-15,14.2469894704645,41.5000000000007));
#5686=CARTESIAN_POINT('',(2.73292925444663E-15,12.2469894704645,55.4465750063058));
#5687=CARTESIAN_POINT('Origin',(2.48799989461716E-15,12.2469894704645,57.4465750063058));
#5688=CARTESIAN_POINT('Origin',(4.44089209850063E-15,12.2469894704645,41.5000000000007));
#5689=CARTESIAN_POINT('Origin',(4.44089209850063E-15,7.53774265117334,41.5000000000007));
#5690=CARTESIAN_POINT('',(2.73292925444663E-15,2.82849583188222,55.4465750063058));
#5691=CARTESIAN_POINT('Origin',(4.44089209850063E-15,2.82849583188222,41.5000000000007));
#5692=CARTESIAN_POINT('',(2.73292925444663E-15,7.53774265117334,55.4465750063058));
#5693=CARTESIAN_POINT('Origin',(4.44089209850063E-15,14.2469894704645,27.5534249936957));
#5694=CARTESIAN_POINT('',(7.86803243093589E-16,14.2469894704645,71.3378998577488));
#5695=CARTESIAN_POINT('Origin',(4.44089209850063E-15,14.2469894704645,41.5000000000007));
#5696=CARTESIAN_POINT('Origin',(4.44089209850063E-15,2.82849583188222,41.5000000000007));
#5697=CARTESIAN_POINT('',(2.9778586142761E-15,0.828495831882226,53.4465750063058));
#5698=CARTESIAN_POINT('Origin',(4.44089209850063E-15,0.828495831882226,
41.5000000000007));
#5699=CARTESIAN_POINT('Origin',(2.9778586142761E-15,2.82849583188222,53.4465750063058));
#5700=CARTESIAN_POINT('Origin',(4.44089209850063E-15,0.828495831882226,
41.5000000000007));
#5701=CARTESIAN_POINT('Origin',(4.44089209850063E-15,16.2469894704645,41.5000000000007));
#5702=CARTESIAN_POINT('Origin',(7.86803243093589E-16,16.2469894704645,71.3378998577488));
#5703=CARTESIAN_POINT('Origin',(4.44089209850063E-15,26.3469309188597,41.5000000000007));
#5704=CARTESIAN_POINT('',(-7.65691650535287E-17,26.3469309188597,78.3878705819464));
#5705=CARTESIAN_POINT('Origin',(1.68360194775942E-16,26.3469309188597,76.3878705819464));
#5706=CARTESIAN_POINT('Origin',(4.44089209850063E-15,26.3469309188597,41.5000000000007));
#5707=CARTESIAN_POINT('Origin',(4.44089209850063E-15,30.673456552356,41.5000000000007));
#5708=CARTESIAN_POINT('',(-7.65691650535287E-17,36.9999821858522,78.3878705819464));
#5709=CARTESIAN_POINT('',(-7.65691650535287E-17,30.673456552356,78.3878705819464));
#5710=CARTESIAN_POINT('Origin',(4.44089209850063E-15,36.9999821858522,41.5000000000007));
#5711=CARTESIAN_POINT('Origin',(4.44089209850063E-15,36.9999821858522,4.6121294180551));
#5712=CARTESIAN_POINT('',(0.,0.,0.));
#5713=CARTESIAN_POINT('Origin',(-31.6092837386808,245.5,108.939950998448));
#5714=CARTESIAN_POINT('',(-33.6092837386808,242.5,108.939950998448));
#5715=CARTESIAN_POINT('Origin',(-31.6092837386808,242.5,108.939950998448));
#5716=CARTESIAN_POINT('',(-33.6092837386808,245.5,108.939950998448));
#5717=CARTESIAN_POINT('',(-33.6092837386808,245.5,108.939950998448));
#5718=CARTESIAN_POINT('Origin',(-31.6092837386808,245.5,108.939950998448));
#5719=CARTESIAN_POINT('Origin',(-71.0061608111161,245.5,95.0000000000015));
#5720=CARTESIAN_POINT('',(-73.0061608111161,242.5,95.0000000000015));
#5721=CARTESIAN_POINT('Origin',(-71.0061608111161,242.5,95.0000000000015));
#5722=CARTESIAN_POINT('',(-73.0061608111161,245.5,95.0000000000015));
#5723=CARTESIAN_POINT('',(-73.0061608111161,245.5,95.0000000000015));
#5724=CARTESIAN_POINT('Origin',(-71.0061608111161,245.5,95.0000000000015));
#5725=CARTESIAN_POINT('Origin',(-28.0061608111161,245.5,95.0000000000015));
#5726=CARTESIAN_POINT('',(-30.0061608111161,242.5,95.0000000000015));
#5727=CARTESIAN_POINT('Origin',(-28.0061608111161,242.5,95.0000000000015));
#5728=CARTESIAN_POINT('',(-30.0061608111161,245.5,95.0000000000015));
#5729=CARTESIAN_POINT('',(-30.0061608111161,245.5,95.0000000000015));
#5730=CARTESIAN_POINT('Origin',(-28.0061608111161,245.5,95.0000000000015));
#5731=CARTESIAN_POINT('Origin',(-67.4030378835514,245.5,108.939950998448));
#5732=CARTESIAN_POINT('',(-69.4030378835514,242.5,108.939950998448));
#5733=CARTESIAN_POINT('Origin',(-67.4030378835514,242.5,108.939950998448));
#5734=CARTESIAN_POINT('',(-69.4030378835514,245.5,108.939950998448));
#5735=CARTESIAN_POINT('',(-69.4030378835514,245.5,108.939950998448));
#5736=CARTESIAN_POINT('Origin',(-67.4030378835514,245.5,108.939950998448));
#5737=CARTESIAN_POINT('Origin',(-67.5061608111161,245.5,105.000000000001));
#5738=CARTESIAN_POINT('',(-67.5061608111161,245.5,105.000000000001));
#5739=CARTESIAN_POINT('',(-31.5061608111161,245.5,105.000000000001));
#5740=CARTESIAN_POINT('',(-67.5061608111161,245.5,105.000000000001));
#5741=CARTESIAN_POINT('',(-31.5061608111161,242.5,105.000000000001));
#5742=CARTESIAN_POINT('',(-31.5061608111161,245.5,105.000000000001));
#5743=CARTESIAN_POINT('',(-67.5061608111161,242.5,105.000000000001));
#5744=CARTESIAN_POINT('',(-67.5061608111161,242.5,105.000000000001));
#5745=CARTESIAN_POINT('',(-67.5061608111161,245.5,105.000000000001));
#5746=CARTESIAN_POINT('Origin',(-67.5061608111161,245.5,85.0000000000015));
#5747=CARTESIAN_POINT('',(-67.5061608111161,245.5,85.0000000000015));
#5748=CARTESIAN_POINT('',(-67.5061608111161,245.5,85.0000000000015));
#5749=CARTESIAN_POINT('',(-67.5061608111161,242.5,85.0000000000015));
#5750=CARTESIAN_POINT('',(-67.5061608111161,242.5,85.0000000000015));
#5751=CARTESIAN_POINT('',(-67.5061608111161,245.5,85.0000000000015));
#5752=CARTESIAN_POINT('Origin',(-51.5061608111161,245.5,85.0000000000015));
#5753=CARTESIAN_POINT('',(-51.5061608111161,245.5,85.0000000000015));
#5754=CARTESIAN_POINT('',(-31.5061608111161,245.5,85.0000000000015));
#5755=CARTESIAN_POINT('',(-51.5061608111161,242.5,85.0000000000015));
#5756=CARTESIAN_POINT('',(-31.5061608111161,242.5,85.0000000000015));
#5757=CARTESIAN_POINT('',(-51.5061608111161,245.5,85.0000000000015));
#5758=CARTESIAN_POINT('Origin',(-51.5061608111161,245.5,77.5000000000015));
#5759=CARTESIAN_POINT('',(-51.5061608111161,245.5,77.5000000000015));
#5760=CARTESIAN_POINT('',(-51.5061608111161,245.5,65.0000000000015));
#5761=CARTESIAN_POINT('',(-51.5061608111161,242.5,77.5000000000015));
#5762=CARTESIAN_POINT('',(-51.5061608111161,242.5,65.0000000000015));
#5763=CARTESIAN_POINT('',(-51.5061608111161,245.5,77.5000000000015));
#5764=CARTESIAN_POINT('Origin',(-74.5061608111161,245.5,77.5000000000015));
#5765=CARTESIAN_POINT('',(-74.5061608111161,245.5,77.5000000000015));
#5766=CARTESIAN_POINT('',(-74.5061608111161,245.5,77.5000000000015));
#5767=CARTESIAN_POINT('',(-74.5061608111161,242.5,77.5000000000015));
#5768=CARTESIAN_POINT('',(-74.5061608111161,242.5,77.5000000000015));
#5769=CARTESIAN_POINT('',(-74.5061608111161,245.5,77.5000000000015));
#5770=CARTESIAN_POINT('Origin',(-74.5061608111161,245.5,112.500000000001));
#5771=CARTESIAN_POINT('',(-74.5061608111161,245.5,112.500000000001));
#5772=CARTESIAN_POINT('',(-74.5061608111161,245.5,112.500000000001));
#5773=CARTESIAN_POINT('',(-74.5061608111161,242.5,112.500000000001));
#5774=CARTESIAN_POINT('',(-74.5061608111161,242.5,112.500000000001));
#5775=CARTESIAN_POINT('',(-74.5061608111161,245.5,112.500000000001));
#5776=CARTESIAN_POINT('Origin',(-24.5061608111161,245.5,112.500000000001));
#5777=CARTESIAN_POINT('',(-24.5061608111161,245.5,112.500000000001));
#5778=CARTESIAN_POINT('',(-24.5061608111161,245.5,112.500000000001));
#5779=CARTESIAN_POINT('',(-24.5061608111161,242.5,112.500000000001));
#5780=CARTESIAN_POINT('',(-24.5061608111161,242.5,112.500000000001));
#5781=CARTESIAN_POINT('',(-24.5061608111161,245.5,112.500000000001));
#5782=CARTESIAN_POINT('Origin',(-24.5061608111161,245.5,77.5000000000015));
#5783=CARTESIAN_POINT('',(-24.5061608111161,245.5,77.5000000000015));
#5784=CARTESIAN_POINT('',(-24.5061608111161,245.5,77.5000000000015));
#5785=CARTESIAN_POINT('',(-24.5061608111161,242.5,77.5000000000015));
#5786=CARTESIAN_POINT('',(-24.5061608111161,242.5,77.5000000000015));
#5787=CARTESIAN_POINT('',(-24.5061608111161,245.5,77.5000000000015));
#5788=CARTESIAN_POINT('Origin',(-31.5061608111161,245.5,77.5000000000015));
#5789=CARTESIAN_POINT('',(-31.5061608111161,245.5,77.5000000000015));
#5790=CARTESIAN_POINT('',(-74.5061608111161,245.5,77.5000000000015));
#5791=CARTESIAN_POINT('',(-31.5061608111161,242.5,77.5000000000015));
#5792=CARTESIAN_POINT('',(-74.5061608111161,242.5,77.5000000000015));
#5793=CARTESIAN_POINT('',(-31.5061608111161,245.5,77.5000000000015));
#5794=CARTESIAN_POINT('Origin',(-31.5061608111161,245.5,105.000000000001));
#5795=CARTESIAN_POINT('',(-31.5061608111161,245.5,85.0000000000015));
#5796=CARTESIAN_POINT('',(-31.5061608111161,242.5,85.0000000000015));
#5797=CARTESIAN_POINT('Origin',(-49.5061608111161,242.5,95.0000000000015));
#5798=CARTESIAN_POINT('Origin',(-49.5061608111161,245.5,95.0000000000015));
#5799=CARTESIAN_POINT('',(0.,0.,0.));
#5800=CARTESIAN_POINT('Origin',(31.6092837386808,245.5,108.939950998448));
#5801=CARTESIAN_POINT('',(33.6092837386808,242.5,108.939950998448));
#5802=CARTESIAN_POINT('Origin',(31.6092837386808,242.5,108.939950998448));
#5803=CARTESIAN_POINT('',(33.6092837386808,245.5,108.939950998448));
#5804=CARTESIAN_POINT('',(33.6092837386808,245.5,108.939950998448));
#5805=CARTESIAN_POINT('Origin',(31.6092837386808,245.5,108.939950998448));
#5806=CARTESIAN_POINT('Origin',(71.0061608111161,245.5,95.0000000000015));
#5807=CARTESIAN_POINT('',(73.0061608111161,242.5,95.0000000000015));
#5808=CARTESIAN_POINT('Origin',(71.0061608111161,242.5,95.0000000000015));
#5809=CARTESIAN_POINT('',(73.0061608111161,245.5,95.0000000000015));
#5810=CARTESIAN_POINT('',(73.0061608111161,245.5,95.0000000000015));
#5811=CARTESIAN_POINT('Origin',(71.0061608111161,245.5,95.0000000000015));
#5812=CARTESIAN_POINT('Origin',(28.0061608111161,245.5,95.0000000000015));
#5813=CARTESIAN_POINT('',(30.0061608111161,242.5,95.0000000000015));
#5814=CARTESIAN_POINT('Origin',(28.0061608111161,242.5,95.0000000000015));
#5815=CARTESIAN_POINT('',(30.0061608111161,245.5,95.0000000000015));
#5816=CARTESIAN_POINT('',(30.0061608111161,245.5,95.0000000000015));
#5817=CARTESIAN_POINT('Origin',(28.0061608111161,245.5,95.0000000000015));
#5818=CARTESIAN_POINT('Origin',(67.4030378835514,245.5,108.939950998448));
#5819=CARTESIAN_POINT('',(69.4030378835514,242.5,108.939950998448));
#5820=CARTESIAN_POINT('Origin',(67.4030378835514,242.5,108.939950998448));
#5821=CARTESIAN_POINT('',(69.4030378835514,245.5,108.939950998448));
#5822=CARTESIAN_POINT('',(69.4030378835514,245.5,108.939950998448));
#5823=CARTESIAN_POINT('Origin',(67.4030378835514,245.5,108.939950998448));
#5824=CARTESIAN_POINT('Origin',(67.5061608111161,245.5,105.000000000001));
#5825=CARTESIAN_POINT('',(67.5061608111161,245.5,105.000000000001));
#5826=CARTESIAN_POINT('',(31.5061608111161,245.5,105.000000000001));
#5827=CARTESIAN_POINT('',(67.5061608111161,245.5,105.000000000001));
#5828=CARTESIAN_POINT('',(67.5061608111161,242.5,105.000000000001));
#5829=CARTESIAN_POINT('',(67.5061608111161,245.5,105.000000000001));
#5830=CARTESIAN_POINT('',(31.5061608111161,242.5,105.000000000001));
#5831=CARTESIAN_POINT('',(67.5061608111161,242.5,105.000000000001));
#5832=CARTESIAN_POINT('',(31.5061608111161,245.5,105.000000000001));
#5833=CARTESIAN_POINT('Origin',(67.5061608111161,245.5,85.0000000000015));
#5834=CARTESIAN_POINT('',(67.5061608111161,245.5,85.0000000000015));
#5835=CARTESIAN_POINT('',(67.5061608111161,245.5,85.0000000000015));
#5836=CARTESIAN_POINT('',(67.5061608111161,242.5,85.0000000000015));
#5837=CARTESIAN_POINT('',(67.5061608111161,245.5,85.0000000000015));
#5838=CARTESIAN_POINT('',(67.5061608111161,242.5,85.0000000000015));
#5839=CARTESIAN_POINT('Origin',(51.5061608111161,245.5,85.0000000000015));
#5840=CARTESIAN_POINT('',(51.5061608111161,245.5,85.0000000000015));
#5841=CARTESIAN_POINT('',(31.5061608111161,245.5,85.0000000000015));
#5842=CARTESIAN_POINT('',(51.5061608111161,242.5,85.0000000000015));
#5843=CARTESIAN_POINT('',(51.5061608111161,245.5,85.0000000000015));
#5844=CARTESIAN_POINT('',(31.5061608111161,242.5,85.0000000000015));
#5845=CARTESIAN_POINT('Origin',(51.5061608111161,245.5,77.5000000000015));
#5846=CARTESIAN_POINT('',(51.5061608111161,245.5,77.5000000000015));
#5847=CARTESIAN_POINT('',(51.5061608111161,245.5,65.0000000000015));
#5848=CARTESIAN_POINT('',(51.5061608111161,242.5,77.5000000000015));
#5849=CARTESIAN_POINT('',(51.5061608111161,245.5,77.5000000000015));
#5850=CARTESIAN_POINT('',(51.5061608111161,242.5,65.0000000000015));
#5851=CARTESIAN_POINT('Origin',(74.5061608111161,245.5,77.5000000000015));
#5852=CARTESIAN_POINT('',(74.5061608111161,245.5,77.5000000000015));
#5853=CARTESIAN_POINT('',(74.5061608111161,245.5,77.5000000000015));
#5854=CARTESIAN_POINT('',(74.5061608111161,242.5,77.5000000000015));
#5855=CARTESIAN_POINT('',(74.5061608111161,245.5,77.5000000000015));
#5856=CARTESIAN_POINT('',(74.5061608111161,242.5,77.5000000000015));
#5857=CARTESIAN_POINT('Origin',(74.5061608111161,245.5,112.500000000001));
#5858=CARTESIAN_POINT('',(74.5061608111161,245.5,112.500000000001));
#5859=CARTESIAN_POINT('',(74.5061608111161,245.5,112.500000000001));
#5860=CARTESIAN_POINT('',(74.5061608111161,242.5,112.500000000001));
#5861=CARTESIAN_POINT('',(74.5061608111161,245.5,112.500000000001));
#5862=CARTESIAN_POINT('',(74.5061608111161,242.5,112.500000000001));
#5863=CARTESIAN_POINT('Origin',(24.5061608111161,245.5,112.500000000001));
#5864=CARTESIAN_POINT('',(24.5061608111161,245.5,112.500000000001));
#5865=CARTESIAN_POINT('',(24.5061608111161,245.5,112.500000000001));
#5866=CARTESIAN_POINT('',(24.5061608111161,242.5,112.500000000001));
#5867=CARTESIAN_POINT('',(24.5061608111161,245.5,112.500000000001));
#5868=CARTESIAN_POINT('',(24.5061608111161,242.5,112.500000000001));
#5869=CARTESIAN_POINT('Origin',(24.5061608111161,245.5,77.5000000000015));
#5870=CARTESIAN_POINT('',(24.5061608111161,245.5,77.5000000000015));
#5871=CARTESIAN_POINT('',(24.5061608111161,245.5,77.5000000000015));
#5872=CARTESIAN_POINT('',(24.5061608111161,242.5,77.5000000000015));
#5873=CARTESIAN_POINT('',(24.5061608111161,245.5,77.5000000000015));
#5874=CARTESIAN_POINT('',(24.5061608111161,242.5,77.5000000000015));
#5875=CARTESIAN_POINT('Origin',(31.5061608111161,245.5,77.5000000000015));
#5876=CARTESIAN_POINT('',(31.5061608111161,245.5,77.5000000000015));
#5877=CARTESIAN_POINT('',(74.5061608111161,245.5,77.5000000000015));
#5878=CARTESIAN_POINT('',(31.5061608111161,242.5,77.5000000000015));
#5879=CARTESIAN_POINT('',(31.5061608111161,245.5,77.5000000000015));
#5880=CARTESIAN_POINT('',(74.5061608111161,242.5,77.5000000000015));
#5881=CARTESIAN_POINT('Origin',(31.5061608111161,245.5,105.000000000001));
#5882=CARTESIAN_POINT('',(31.5061608111161,245.5,85.0000000000015));
#5883=CARTESIAN_POINT('',(31.5061608111161,242.5,85.0000000000015));
#5884=CARTESIAN_POINT('Origin',(49.5061608111161,242.5,95.0000000000015));
#5885=CARTESIAN_POINT('Origin',(49.5061608111161,245.5,95.0000000000015));
#5886=CARTESIAN_POINT('',(0.,0.,0.));
#5887=CARTESIAN_POINT('Origin',(-31.6092837386808,460.5,108.939950998448));
#5888=CARTESIAN_POINT('',(-33.6092837386808,463.5,108.939950998448));
#5889=CARTESIAN_POINT('Origin',(-31.6092837386808,463.5,108.939950998448));
#5890=CARTESIAN_POINT('',(-33.6092837386808,460.5,108.939950998448));
#5891=CARTESIAN_POINT('',(-33.6092837386808,460.5,108.939950998448));
#5892=CARTESIAN_POINT('Origin',(-31.6092837386808,460.5,108.939950998448));
#5893=CARTESIAN_POINT('Origin',(-71.0061608111161,460.5,95.0000000000015));
#5894=CARTESIAN_POINT('',(-73.0061608111161,463.5,95.0000000000015));
#5895=CARTESIAN_POINT('Origin',(-71.0061608111161,463.5,95.0000000000015));
#5896=CARTESIAN_POINT('',(-73.0061608111161,460.5,95.0000000000015));
#5897=CARTESIAN_POINT('',(-73.0061608111161,460.5,95.0000000000015));
#5898=CARTESIAN_POINT('Origin',(-71.0061608111161,460.5,95.0000000000015));
#5899=CARTESIAN_POINT('Origin',(-28.0061608111161,460.5,95.0000000000015));
#5900=CARTESIAN_POINT('',(-30.0061608111161,463.5,95.0000000000015));
#5901=CARTESIAN_POINT('Origin',(-28.0061608111161,463.5,95.0000000000015));
#5902=CARTESIAN_POINT('',(-30.0061608111161,460.5,95.0000000000015));
#5903=CARTESIAN_POINT('',(-30.0061608111161,460.5,95.0000000000015));
#5904=CARTESIAN_POINT('Origin',(-28.0061608111161,460.5,95.0000000000015));
#5905=CARTESIAN_POINT('Origin',(-67.4030378835514,460.5,108.939950998448));
#5906=CARTESIAN_POINT('',(-69.4030378835514,463.5,108.939950998448));
#5907=CARTESIAN_POINT('Origin',(-67.4030378835514,463.5,108.939950998448));
#5908=CARTESIAN_POINT('',(-69.4030378835514,460.5,108.939950998448));
#5909=CARTESIAN_POINT('',(-69.4030378835514,460.5,108.939950998448));
#5910=CARTESIAN_POINT('Origin',(-67.4030378835514,460.5,108.939950998448));
#5911=CARTESIAN_POINT('Origin',(-67.5061608111161,460.5,105.000000000001));
#5912=CARTESIAN_POINT('',(-67.5061608111161,460.5,105.000000000001));
#5913=CARTESIAN_POINT('',(-31.5061608111161,460.5,105.000000000001));
#5914=CARTESIAN_POINT('',(-67.5061608111161,460.5,105.000000000001));
#5915=CARTESIAN_POINT('',(-67.5061608111161,463.5,105.000000000001));
#5916=CARTESIAN_POINT('',(-67.5061608111161,460.5,105.000000000001));
#5917=CARTESIAN_POINT('',(-31.5061608111161,463.5,105.000000000001));
#5918=CARTESIAN_POINT('',(-67.5061608111161,463.5,105.000000000001));
#5919=CARTESIAN_POINT('',(-31.5061608111161,460.5,105.000000000001));
#5920=CARTESIAN_POINT('Origin',(-67.5061608111161,460.5,85.0000000000015));
#5921=CARTESIAN_POINT('',(-67.5061608111161,460.5,85.0000000000015));
#5922=CARTESIAN_POINT('',(-67.5061608111161,460.5,85.0000000000015));
#5923=CARTESIAN_POINT('',(-67.5061608111161,463.5,85.0000000000015));
#5924=CARTESIAN_POINT('',(-67.5061608111161,460.5,85.0000000000015));
#5925=CARTESIAN_POINT('',(-67.5061608111161,463.5,85.0000000000015));
#5926=CARTESIAN_POINT('Origin',(-51.5061608111161,460.5,85.0000000000015));
#5927=CARTESIAN_POINT('',(-51.5061608111161,460.5,85.0000000000015));
#5928=CARTESIAN_POINT('',(-31.5061608111161,460.5,85.0000000000015));
#5929=CARTESIAN_POINT('',(-51.5061608111161,463.5,85.0000000000015));
#5930=CARTESIAN_POINT('',(-51.5061608111161,460.5,85.0000000000015));
#5931=CARTESIAN_POINT('',(-31.5061608111161,463.5,85.0000000000015));
#5932=CARTESIAN_POINT('Origin',(-51.5061608111161,460.5,77.5000000000015));
#5933=CARTESIAN_POINT('',(-51.5061608111161,460.5,77.5000000000015));
#5934=CARTESIAN_POINT('',(-51.5061608111161,460.5,65.0000000000015));
#5935=CARTESIAN_POINT('',(-51.5061608111161,463.5,77.5000000000015));
#5936=CARTESIAN_POINT('',(-51.5061608111161,460.5,77.5000000000015));
#5937=CARTESIAN_POINT('',(-51.5061608111161,463.5,65.0000000000015));
#5938=CARTESIAN_POINT('Origin',(-74.5061608111161,460.5,77.5000000000015));
#5939=CARTESIAN_POINT('',(-74.5061608111161,460.5,77.5000000000015));
#5940=CARTESIAN_POINT('',(-74.5061608111161,460.5,77.5000000000015));
#5941=CARTESIAN_POINT('',(-74.5061608111161,463.5,77.5000000000015));
#5942=CARTESIAN_POINT('',(-74.5061608111161,460.5,77.5000000000015));
#5943=CARTESIAN_POINT('',(-74.5061608111161,463.5,77.5000000000015));
#5944=CARTESIAN_POINT('Origin',(-74.5061608111161,460.5,112.500000000001));
#5945=CARTESIAN_POINT('',(-74.5061608111161,460.5,112.500000000001));
#5946=CARTESIAN_POINT('',(-74.5061608111161,460.5,112.500000000001));
#5947=CARTESIAN_POINT('',(-74.5061608111161,463.5,112.500000000001));
#5948=CARTESIAN_POINT('',(-74.5061608111161,460.5,112.500000000001));
#5949=CARTESIAN_POINT('',(-74.5061608111161,463.5,112.500000000001));
#5950=CARTESIAN_POINT('Origin',(-24.5061608111161,460.5,112.500000000001));
#5951=CARTESIAN_POINT('',(-24.5061608111161,460.5,112.500000000001));
#5952=CARTESIAN_POINT('',(-24.5061608111161,460.5,112.500000000001));
#5953=CARTESIAN_POINT('',(-24.5061608111161,463.5,112.500000000001));
#5954=CARTESIAN_POINT('',(-24.5061608111161,460.5,112.500000000001));
#5955=CARTESIAN_POINT('',(-24.5061608111161,463.5,112.500000000001));
#5956=CARTESIAN_POINT('Origin',(-24.5061608111161,460.5,77.5000000000015));
#5957=CARTESIAN_POINT('',(-24.5061608111161,460.5,77.5000000000015));
#5958=CARTESIAN_POINT('',(-24.5061608111161,460.5,77.5000000000015));
#5959=CARTESIAN_POINT('',(-24.5061608111161,463.5,77.5000000000015));
#5960=CARTESIAN_POINT('',(-24.5061608111161,460.5,77.5000000000015));
#5961=CARTESIAN_POINT('',(-24.5061608111161,463.5,77.5000000000015));
#5962=CARTESIAN_POINT('Origin',(-31.5061608111161,460.5,77.5000000000015));
#5963=CARTESIAN_POINT('',(-31.5061608111161,460.5,77.5000000000015));
#5964=CARTESIAN_POINT('',(-74.5061608111161,460.5,77.5000000000015));
#5965=CARTESIAN_POINT('',(-31.5061608111161,463.5,77.5000000000015));
#5966=CARTESIAN_POINT('',(-31.5061608111161,460.5,77.5000000000015));
#5967=CARTESIAN_POINT('',(-74.5061608111161,463.5,77.5000000000015));
#5968=CARTESIAN_POINT('Origin',(-31.5061608111161,460.5,105.000000000001));
#5969=CARTESIAN_POINT('',(-31.5061608111161,460.5,85.0000000000015));
#5970=CARTESIAN_POINT('',(-31.5061608111161,463.5,85.0000000000015));
#5971=CARTESIAN_POINT('Origin',(-49.5061608111161,463.5,95.0000000000015));
#5972=CARTESIAN_POINT('Origin',(-49.5061608111161,460.5,95.0000000000015));
#5973=CARTESIAN_POINT('',(0.,0.,0.));
#5974=CARTESIAN_POINT('Origin',(31.6092837386808,460.5,108.939950998448));
#5975=CARTESIAN_POINT('',(33.6092837386808,463.5,108.939950998448));
#5976=CARTESIAN_POINT('Origin',(31.6092837386808,463.5,108.939950998448));
#5977=CARTESIAN_POINT('',(33.6092837386808,460.5,108.939950998448));
#5978=CARTESIAN_POINT('',(33.6092837386808,460.5,108.939950998448));
#5979=CARTESIAN_POINT('Origin',(31.6092837386808,460.5,108.939950998448));
#5980=CARTESIAN_POINT('Origin',(71.0061608111161,460.5,95.0000000000015));
#5981=CARTESIAN_POINT('',(73.0061608111161,463.5,95.0000000000015));
#5982=CARTESIAN_POINT('Origin',(71.0061608111161,463.5,95.0000000000015));
#5983=CARTESIAN_POINT('',(73.0061608111161,460.5,95.0000000000015));
#5984=CARTESIAN_POINT('',(73.0061608111161,460.5,95.0000000000015));
#5985=CARTESIAN_POINT('Origin',(71.0061608111161,460.5,95.0000000000015));
#5986=CARTESIAN_POINT('Origin',(28.0061608111161,460.5,95.0000000000015));
#5987=CARTESIAN_POINT('',(30.0061608111161,463.5,95.0000000000015));
#5988=CARTESIAN_POINT('Origin',(28.0061608111161,463.5,95.0000000000015));
#5989=CARTESIAN_POINT('',(30.0061608111161,460.5,95.0000000000015));
#5990=CARTESIAN_POINT('',(30.0061608111161,460.5,95.0000000000015));
#5991=CARTESIAN_POINT('Origin',(28.0061608111161,460.5,95.0000000000015));
#5992=CARTESIAN_POINT('Origin',(67.4030378835514,460.5,108.939950998448));
#5993=CARTESIAN_POINT('',(69.4030378835514,463.5,108.939950998448));
#5994=CARTESIAN_POINT('Origin',(67.4030378835514,463.5,108.939950998448));
#5995=CARTESIAN_POINT('',(69.4030378835514,460.5,108.939950998448));
#5996=CARTESIAN_POINT('',(69.4030378835514,460.5,108.939950998448));
#5997=CARTESIAN_POINT('Origin',(67.4030378835514,460.5,108.939950998448));
#5998=CARTESIAN_POINT('Origin',(67.5061608111161,460.5,105.000000000001));
#5999=CARTESIAN_POINT('',(67.5061608111161,460.5,105.000000000001));
#6000=CARTESIAN_POINT('',(31.5061608111161,460.5,105.000000000001));
#6001=CARTESIAN_POINT('',(67.5061608111161,460.5,105.000000000001));
#6002=CARTESIAN_POINT('',(31.5061608111161,463.5,105.000000000001));
#6003=CARTESIAN_POINT('',(31.5061608111161,460.5,105.000000000001));
#6004=CARTESIAN_POINT('',(67.5061608111161,463.5,105.000000000001));
#6005=CARTESIAN_POINT('',(67.5061608111161,463.5,105.000000000001));
#6006=CARTESIAN_POINT('',(67.5061608111161,460.5,105.000000000001));
#6007=CARTESIAN_POINT('Origin',(67.5061608111161,460.5,85.0000000000015));
#6008=CARTESIAN_POINT('',(67.5061608111161,460.5,85.0000000000015));
#6009=CARTESIAN_POINT('',(67.5061608111161,460.5,85.0000000000015));
#6010=CARTESIAN_POINT('',(67.5061608111161,463.5,85.0000000000015));
#6011=CARTESIAN_POINT('',(67.5061608111161,463.5,85.0000000000015));
#6012=CARTESIAN_POINT('',(67.5061608111161,460.5,85.0000000000015));
#6013=CARTESIAN_POINT('Origin',(51.5061608111161,460.5,85.0000000000015));
#6014=CARTESIAN_POINT('',(51.5061608111161,460.5,85.0000000000015));
#6015=CARTESIAN_POINT('',(31.5061608111161,460.5,85.0000000000015));
#6016=CARTESIAN_POINT('',(51.5061608111161,463.5,85.0000000000015));
#6017=CARTESIAN_POINT('',(31.5061608111161,463.5,85.0000000000015));
#6018=CARTESIAN_POINT('',(51.5061608111161,460.5,85.0000000000015));
#6019=CARTESIAN_POINT('Origin',(51.5061608111161,460.5,77.5000000000015));
#6020=CARTESIAN_POINT('',(51.5061608111161,460.5,77.5000000000015));
#6021=CARTESIAN_POINT('',(51.5061608111161,460.5,65.0000000000015));
#6022=CARTESIAN_POINT('',(51.5061608111161,463.5,77.5000000000015));
#6023=CARTESIAN_POINT('',(51.5061608111161,463.5,65.0000000000015));
#6024=CARTESIAN_POINT('',(51.5061608111161,460.5,77.5000000000015));
#6025=CARTESIAN_POINT('Origin',(74.5061608111161,460.5,77.5000000000015));
#6026=CARTESIAN_POINT('',(74.5061608111161,460.5,77.5000000000015));
#6027=CARTESIAN_POINT('',(74.5061608111161,460.5,77.5000000000015));
#6028=CARTESIAN_POINT('',(74.5061608111161,463.5,77.5000000000015));
#6029=CARTESIAN_POINT('',(74.5061608111161,463.5,77.5000000000015));
#6030=CARTESIAN_POINT('',(74.5061608111161,460.5,77.5000000000015));
#6031=CARTESIAN_POINT('Origin',(74.5061608111161,460.5,112.500000000001));
#6032=CARTESIAN_POINT('',(74.5061608111161,460.5,112.500000000001));
#6033=CARTESIAN_POINT('',(74.5061608111161,460.5,112.500000000001));
#6034=CARTESIAN_POINT('',(74.5061608111161,463.5,112.500000000001));
#6035=CARTESIAN_POINT('',(74.5061608111161,463.5,112.500000000001));
#6036=CARTESIAN_POINT('',(74.5061608111161,460.5,112.500000000001));
#6037=CARTESIAN_POINT('Origin',(24.5061608111161,460.5,112.500000000001));
#6038=CARTESIAN_POINT('',(24.5061608111161,460.5,112.500000000001));
#6039=CARTESIAN_POINT('',(24.5061608111161,460.5,112.500000000001));
#6040=CARTESIAN_POINT('',(24.5061608111161,463.5,112.500000000001));
#6041=CARTESIAN_POINT('',(24.5061608111161,463.5,112.500000000001));
#6042=CARTESIAN_POINT('',(24.5061608111161,460.5,112.500000000001));
#6043=CARTESIAN_POINT('Origin',(24.5061608111161,460.5,77.5000000000015));
#6044=CARTESIAN_POINT('',(24.5061608111161,460.5,77.5000000000015));
#6045=CARTESIAN_POINT('',(24.5061608111161,460.5,77.5000000000015));
#6046=CARTESIAN_POINT('',(24.5061608111161,463.5,77.5000000000015));
#6047=CARTESIAN_POINT('',(24.5061608111161,463.5,77.5000000000015));
#6048=CARTESIAN_POINT('',(24.5061608111161,460.5,77.5000000000015));
#6049=CARTESIAN_POINT('Origin',(31.5061608111161,460.5,77.5000000000015));
#6050=CARTESIAN_POINT('',(31.5061608111161,460.5,77.5000000000015));
#6051=CARTESIAN_POINT('',(74.5061608111161,460.5,77.5000000000015));
#6052=CARTESIAN_POINT('',(31.5061608111161,463.5,77.5000000000015));
#6053=CARTESIAN_POINT('',(74.5061608111161,463.5,77.5000000000015));
#6054=CARTESIAN_POINT('',(31.5061608111161,460.5,77.5000000000015));
#6055=CARTESIAN_POINT('Origin',(31.5061608111161,460.5,105.000000000001));
#6056=CARTESIAN_POINT('',(31.5061608111161,460.5,85.0000000000015));
#6057=CARTESIAN_POINT('',(31.5061608111161,463.5,85.0000000000015));
#6058=CARTESIAN_POINT('Origin',(49.5061608111161,463.5,95.0000000000015));
#6059=CARTESIAN_POINT('Origin',(49.5061608111161,460.5,95.0000000000015));
#6060=CARTESIAN_POINT('',(0.,0.,0.));
#6061=CARTESIAN_POINT('',(0.,0.,0.));
#6062=CARTESIAN_POINT('',(0.,0.,0.));
#6063=CARTESIAN_POINT('',(0.,0.,0.));
#6064=CARTESIAN_POINT('',(0.,0.,0.));
#6065=CARTESIAN_POINT('',(0.,0.,0.));
#6066=CARTESIAN_POINT('',(0.,0.,0.));
#6067=CARTESIAN_POINT('',(0.,0.,0.));
#6068=CARTESIAN_POINT('',(0.,0.,0.));
#6069=CARTESIAN_POINT('',(0.,0.,0.));
#6070=CARTESIAN_POINT('',(0.,0.,0.));
#6071=UNCERTAINTY_MEASURE_WITH_UNIT(LENGTH_MEASURE(0.01),#6097,
'DISTANCE_ACCURACY_VALUE',
'Maximum model space distance between geometric entities at asserted c
onnectivities');
#6072=UNCERTAINTY_MEASURE_WITH_UNIT(LENGTH_MEASURE(0.01),#6097,
'DISTANCE_ACCURACY_VALUE',
'Maximum model space distance between geometric entities at asserted c
onnectivities');
#6073=UNCERTAINTY_MEASURE_WITH_UNIT(LENGTH_MEASURE(0.01),#6097,
'DISTANCE_ACCURACY_VALUE',
'Maximum model space distance between geometric entities at asserted c
onnectivities');
#6074=UNCERTAINTY_MEASURE_WITH_UNIT(LENGTH_MEASURE(0.01),#6097,
'DISTANCE_ACCURACY_VALUE',
'Maximum model space distance between geometric entities at asserted c
onnectivities');
#6075=UNCERTAINTY_MEASURE_WITH_UNIT(LENGTH_MEASURE(0.01),#6097,
'DISTANCE_ACCURACY_VALUE',
'Maximum model space distance between geometric entities at asserted c
onnectivities');
#6076=UNCERTAINTY_MEASURE_WITH_UNIT(LENGTH_MEASURE(0.01),#6097,
'DISTANCE_ACCURACY_VALUE',
'Maximum model space distance between geometric entities at asserted c
onnectivities');
#6077=UNCERTAINTY_MEASURE_WITH_UNIT(LENGTH_MEASURE(0.01),#6097,
'DISTANCE_ACCURACY_VALUE',
'Maximum model space distance between geometric entities at asserted c
onnectivities');
#6078=UNCERTAINTY_MEASURE_WITH_UNIT(LENGTH_MEASURE(0.01),#6097,
'DISTANCE_ACCURACY_VALUE',
'Maximum model space distance between geometric entities at asserted c
onnectivities');
#6079=UNCERTAINTY_MEASURE_WITH_UNIT(LENGTH_MEASURE(0.01),#6097,
'DISTANCE_ACCURACY_VALUE',
'Maximum model space distance between geometric entities at asserted c
onnectivities');
#6080=UNCERTAINTY_MEASURE_WITH_UNIT(LENGTH_MEASURE(0.01),#6097,
'DISTANCE_ACCURACY_VALUE',
'Maximum model space distance between geometric entities at asserted c
onnectivities');
#6081=UNCERTAINTY_MEASURE_WITH_UNIT(LENGTH_MEASURE(0.01),#6097,
'DISTANCE_ACCURACY_VALUE',
'Maximum model space distance between geometric entities at asserted c
onnectivities');
#6082=UNCERTAINTY_MEASURE_WITH_UNIT(LENGTH_MEASURE(0.01),#6097,
'DISTANCE_ACCURACY_VALUE',
'Maximum model space distance between geometric entities at asserted c
onnectivities');
#6083=UNCERTAINTY_MEASURE_WITH_UNIT(LENGTH_MEASURE(0.01),#6097,
'DISTANCE_ACCURACY_VALUE',
'Maximum model space distance between geometric entities at asserted c
onnectivities');
#6084=(
GEOMETRIC_REPRESENTATION_CONTEXT(3)
GLOBAL_UNCERTAINTY_ASSIGNED_CONTEXT((#6071))
GLOBAL_UNIT_ASSIGNED_CONTEXT((#6097,#6099,#6100))
REPRESENTATION_CONTEXT('','3D')
);
#6085=(
GEOMETRIC_REPRESENTATION_CONTEXT(3)
GLOBAL_UNCERTAINTY_ASSIGNED_CONTEXT((#6072))
GLOBAL_UNIT_ASSIGNED_CONTEXT((#6097,#6099,#6100))
REPRESENTATION_CONTEXT('','3D')
);
#6086=(
GEOMETRIC_REPRESENTATION_CONTEXT(3)
GLOBAL_UNCERTAINTY_ASSIGNED_CONTEXT((#6073))
GLOBAL_UNIT_ASSIGNED_CONTEXT((#6097,#6099,#6100))
REPRESENTATION_CONTEXT('','3D')
);
#6087=(
GEOMETRIC_REPRESENTATION_CONTEXT(3)
GLOBAL_UNCERTAINTY_ASSIGNED_CONTEXT((#6074))
GLOBAL_UNIT_ASSIGNED_CONTEXT((#6097,#6099,#6100))
REPRESENTATION_CONTEXT('','3D')
);
#6088=(
GEOMETRIC_REPRESENTATION_CONTEXT(3)
GLOBAL_UNCERTAINTY_ASSIGNED_CONTEXT((#6075))
GLOBAL_UNIT_ASSIGNED_CONTEXT((#6097,#6099,#6100))
REPRESENTATION_CONTEXT('','3D')
);
#6089=(
GEOMETRIC_REPRESENTATION_CONTEXT(3)
GLOBAL_UNCERTAINTY_ASSIGNED_CONTEXT((#6076))
GLOBAL_UNIT_ASSIGNED_CONTEXT((#6097,#6099,#6100))
REPRESENTATION_CONTEXT('','3D')
);
#6090=(
GEOMETRIC_REPRESENTATION_CONTEXT(3)
GLOBAL_UNCERTAINTY_ASSIGNED_CONTEXT((#6077))
GLOBAL_UNIT_ASSIGNED_CONTEXT((#6097,#6099,#6100))
REPRESENTATION_CONTEXT('','3D')
);
#6091=(
GEOMETRIC_REPRESENTATION_CONTEXT(3)
GLOBAL_UNCERTAINTY_ASSIGNED_CONTEXT((#6078))
GLOBAL_UNIT_ASSIGNED_CONTEXT((#6097,#6099,#6100))
REPRESENTATION_CONTEXT('','3D')
);
#6092=(
GEOMETRIC_REPRESENTATION_CONTEXT(3)
GLOBAL_UNCERTAINTY_ASSIGNED_CONTEXT((#6079))
GLOBAL_UNIT_ASSIGNED_CONTEXT((#6097,#6099,#6100))
REPRESENTATION_CONTEXT('','3D')
);
#6093=(
GEOMETRIC_REPRESENTATION_CONTEXT(3)
GLOBAL_UNCERTAINTY_ASSIGNED_CONTEXT((#6080))
GLOBAL_UNIT_ASSIGNED_CONTEXT((#6097,#6099,#6100))
REPRESENTATION_CONTEXT('','3D')
);
#6094=(
GEOMETRIC_REPRESENTATION_CONTEXT(3)
GLOBAL_UNCERTAINTY_ASSIGNED_CONTEXT((#6081))
GLOBAL_UNIT_ASSIGNED_CONTEXT((#6097,#6099,#6100))
REPRESENTATION_CONTEXT('','3D')
);
#6095=(
GEOMETRIC_REPRESENTATION_CONTEXT(3)
GLOBAL_UNCERTAINTY_ASSIGNED_CONTEXT((#6082))
GLOBAL_UNIT_ASSIGNED_CONTEXT((#6097,#6099,#6100))
REPRESENTATION_CONTEXT('','3D')
);
#6096=(
GEOMETRIC_REPRESENTATION_CONTEXT(3)
GLOBAL_UNCERTAINTY_ASSIGNED_CONTEXT((#6083))
GLOBAL_UNIT_ASSIGNED_CONTEXT((#6097,#6099,#6100))
REPRESENTATION_CONTEXT('','3D')
);
#6097=(
LENGTH_UNIT()
NAMED_UNIT(*)
SI_UNIT(.MILLI.,.METRE.)
);
#6098=(
LENGTH_UNIT()
NAMED_UNIT(*)
SI_UNIT($,.METRE.)
);
#6099=(
NAMED_UNIT(*)
PLANE_ANGLE_UNIT()
SI_UNIT($,.RADIAN.)
);
#6100=(
NAMED_UNIT(*)
SI_UNIT($,.STERADIAN.)
SOLID_ANGLE_UNIT()
);
#6101=SHAPE_DEFINITION_REPRESENTATION(#6113,#6136);
#6102=SHAPE_DEFINITION_REPRESENTATION(#6114,#6137);
#6103=SHAPE_DEFINITION_REPRESENTATION(#6115,#6138);
#6104=SHAPE_DEFINITION_REPRESENTATION(#6116,#6139);
#6105=SHAPE_DEFINITION_REPRESENTATION(#6117,#6140);
#6106=SHAPE_DEFINITION_REPRESENTATION(#6118,#6141);
#6107=SHAPE_DEFINITION_REPRESENTATION(#6119,#6142);
#6108=SHAPE_DEFINITION_REPRESENTATION(#6120,#6143);
#6109=SHAPE_DEFINITION_REPRESENTATION(#6121,#6144);
#6110=SHAPE_DEFINITION_REPRESENTATION(#6122,#6145);
#6111=SHAPE_DEFINITION_REPRESENTATION(#6123,#6146);
#6112=SHAPE_DEFINITION_REPRESENTATION(#6124,#6147);
#6113=PRODUCT_DEFINITION_SHAPE('',$,#6149);
#6114=PRODUCT_DEFINITION_SHAPE('',$,#6150);
#6115=PRODUCT_DEFINITION_SHAPE('',$,#6151);
#6116=PRODUCT_DEFINITION_SHAPE('',$,#6152);
#6117=PRODUCT_DEFINITION_SHAPE('',$,#6153);
#6118=PRODUCT_DEFINITION_SHAPE('',$,#6154);
#6119=PRODUCT_DEFINITION_SHAPE('',$,#6155);
#6120=PRODUCT_DEFINITION_SHAPE('',$,#6156);
#6121=PRODUCT_DEFINITION_SHAPE('',$,#6157);
#6122=PRODUCT_DEFINITION_SHAPE('',$,#6158);
#6123=PRODUCT_DEFINITION_SHAPE('',$,#6159);
#6124=PRODUCT_DEFINITION_SHAPE('',$,#6160);
#6125=PRODUCT_DEFINITION_SHAPE($,$,#44);
#6126=PRODUCT_DEFINITION_SHAPE($,$,#45);
#6127=PRODUCT_DEFINITION_SHAPE($,$,#46);
#6128=PRODUCT_DEFINITION_SHAPE($,$,#47);
#6129=PRODUCT_DEFINITION_SHAPE($,$,#48);
#6130=PRODUCT_DEFINITION_SHAPE($,$,#49);
#6131=PRODUCT_DEFINITION_SHAPE($,$,#50);
#6132=PRODUCT_DEFINITION_SHAPE($,$,#51);
#6133=PRODUCT_DEFINITION_SHAPE($,$,#52);
#6134=PRODUCT_DEFINITION_SHAPE($,$,#53);
#6135=PRODUCT_DEFINITION_SHAPE($,$,#54);
#6136=SHAPE_REPRESENTATION('',(#3726,#4032,#4033,#4034,#4035,#4036,#4037,
#4038,#4039,#4040,#4041,#4042),#6084);
#6137=SHAPE_REPRESENTATION('',(#3727),#6085);
#6138=SHAPE_REPRESENTATION('',(#3789),#6086);
#6139=SHAPE_REPRESENTATION('',(#3806),#6087);
#6140=SHAPE_REPRESENTATION('',(#3856),#6088);
#6141=SHAPE_REPRESENTATION('',(#3875),#6089);
#6142=SHAPE_REPRESENTATION('',(#3885),#6090);
#6143=SHAPE_REPRESENTATION('',(#3903),#6091);
#6144=SHAPE_REPRESENTATION('',(#3932),#6092);
#6145=SHAPE_REPRESENTATION('',(#3957),#6093);
#6146=SHAPE_REPRESENTATION('',(#3982),#6094);
#6147=SHAPE_REPRESENTATION('',(#4007),#6095);
#6148=PRODUCT_DEFINITION_CONTEXT('part definition',#6186,'design');
#6149=PRODUCT_DEFINITION('MAS-277','MAS-277',#6161,#6148);
#6150=PRODUCT_DEFINITION('Base','Base',#6162,#6148);
#6151=PRODUCT_DEFINITION('Coupling','Coupling',#6163,#6148);
#6152=PRODUCT_DEFINITION('Plate','Plate',#6164,#6148);
#6153=PRODUCT_DEFINITION('Motor','Motor',#6165,#6148);
#6154=PRODUCT_DEFINITION('Screw','Screw',#6166,#6148);
#6155=PRODUCT_DEFINITION('Motor_Mount','Motor_Mount',#6167,#6148);
#6156=PRODUCT_DEFINITION('Front_part','Front_part',#6168,#6148);
#6157=PRODUCT_DEFINITION('Bracket_01','Bracket_01',#6169,#6148);
#6158=PRODUCT_DEFINITION('Bracket_02','Bracket_02',#6170,#6148);
#6159=PRODUCT_DEFINITION('Bracket_03','Bracket_03',#6171,#6148);
#6160=PRODUCT_DEFINITION('Bracket_04','Bracket_04',#6172,#6148);
#6161=PRODUCT_DEFINITION_FORMATION('',$,#6188);
#6162=PRODUCT_DEFINITION_FORMATION('',$,#6189);
#6163=PRODUCT_DEFINITION_FORMATION('',$,#6190);
#6164=PRODUCT_DEFINITION_FORMATION('',$,#6191);
#6165=PRODUCT_DEFINITION_FORMATION('',$,#6192);
#6166=PRODUCT_DEFINITION_FORMATION('',$,#6193);
#6167=PRODUCT_DEFINITION_FORMATION('',$,#6194);
#6168=PRODUCT_DEFINITION_FORMATION('',$,#6195);
#6169=PRODUCT_DEFINITION_FORMATION('',$,#6196);
#6170=PRODUCT_DEFINITION_FORMATION('',$,#6197);
#6171=PRODUCT_DEFINITION_FORMATION('',$,#6198);
#6172=PRODUCT_DEFINITION_FORMATION('',$,#6199);
#6173=PRODUCT_RELATED_PRODUCT_CATEGORY('MAS-277','MAS-277',(#6188));
#6174=PRODUCT_RELATED_PRODUCT_CATEGORY('Base','Base',(#6189));
#6175=PRODUCT_RELATED_PRODUCT_CATEGORY('Coupling','Coupling',(#6190));
#6176=PRODUCT_RELATED_PRODUCT_CATEGORY('Plate','Plate',(#6191));
#6177=PRODUCT_RELATED_PRODUCT_CATEGORY('Motor','Motor',(#6192));
#6178=PRODUCT_RELATED_PRODUCT_CATEGORY('Screw','Screw',(#6193));
#6179=PRODUCT_RELATED_PRODUCT_CATEGORY('Motor_Mount','Motor_Mount',(#6194));
#6180=PRODUCT_RELATED_PRODUCT_CATEGORY('Front_part','Front_part',(#6195));
#6181=PRODUCT_RELATED_PRODUCT_CATEGORY('Bracket_01','Bracket_01',(#6196));
#6182=PRODUCT_RELATED_PRODUCT_CATEGORY('Bracket_02','Bracket_02',(#6197));
#6183=PRODUCT_RELATED_PRODUCT_CATEGORY('Bracket_03','Bracket_03',(#6198));
#6184=PRODUCT_RELATED_PRODUCT_CATEGORY('Bracket_04','Bracket_04',(#6199));
#6185=APPLICATION_PROTOCOL_DEFINITION('international standard',
'automotive_design',2009,#6186);
#6186=APPLICATION_CONTEXT(
'Core Data for Automotive Mechanical Design Process');
#6187=PRODUCT_CONTEXT('part definition',#6186,'mechanical');
#6188=PRODUCT('MAS-277','MAS-277',$,(#6187));
#6189=PRODUCT('Base','Base',$,(#6187));
#6190=PRODUCT('Coupling','Coupling',$,(#6187));
#6191=PRODUCT('Plate','Plate',$,(#6187));
#6192=PRODUCT('Motor','Motor',$,(#6187));
#6193=PRODUCT('Screw','Screw',$,(#6187));
#6194=PRODUCT('Motor_Mount','Motor_Mount',$,(#6187));
#6195=PRODUCT('Front_part','Front_part',$,(#6187));
#6196=PRODUCT('Bracket_01','Bracket_01',$,(#6187));
#6197=PRODUCT('Bracket_02','Bracket_02',$,(#6187));
#6198=PRODUCT('Bracket_03','Bracket_03',$,(#6187));
#6199=PRODUCT('Bracket_04','Bracket_04',$,(#6187));
#6200=PRESENTATION_STYLE_ASSIGNMENT((#6204));
#6201=PRESENTATION_STYLE_ASSIGNMENT((#6205));
#6202=PRESENTATION_STYLE_ASSIGNMENT((#6206));
#6203=PRESENTATION_STYLE_ASSIGNMENT((#6207));
#6204=SURFACE_STYLE_USAGE(.BOTH.,#6208);
#6205=SURFACE_STYLE_USAGE(.BOTH.,#6209);
#6206=SURFACE_STYLE_USAGE(.BOTH.,#6210);
#6207=SURFACE_STYLE_USAGE(.BOTH.,#6211);
#6208=SURFACE_SIDE_STYLE('',(#6212));
#6209=SURFACE_SIDE_STYLE('',(#6213));
#6210=SURFACE_SIDE_STYLE('',(#6214));
#6211=SURFACE_SIDE_STYLE('',(#6215));
#6212=SURFACE_STYLE_FILL_AREA(#6216);
#6213=SURFACE_STYLE_FILL_AREA(#6217);
#6214=SURFACE_STYLE_FILL_AREA(#6218);
#6215=SURFACE_STYLE_FILL_AREA(#6219);
#6216=FILL_AREA_STYLE('Steel - Satin',(#6220));
#6217=FILL_AREA_STYLE('Steel - Satin (3)',(#6221));
#6218=FILL_AREA_STYLE('Steel - Satin (1)',(#6222));
#6219=FILL_AREA_STYLE('Steel - Satin (2)',(#6223));
#6220=FILL_AREA_STYLE_COLOUR('Steel - Satin',#6224);
#6221=FILL_AREA_STYLE_COLOUR('Steel - Satin (3)',#6225);
#6222=FILL_AREA_STYLE_COLOUR('Steel - Satin (1)',#6226);
#6223=FILL_AREA_STYLE_COLOUR('Steel - Satin (2)',#6227);
#6224=COLOUR_RGB('Steel - Satin',0.627450980392157,0.627450980392157,0.627450980392157);
#6225=COLOUR_RGB('Steel - Satin (3)',0.32156862745098,0.898039215686275,
0.607843137254902);
#6226=COLOUR_RGB('Steel - Satin (1)',1.,1.,1.);
#6227=COLOUR_RGB('Steel - Satin (2)',0.290196078431373,0.290196078431373,
0.290196078431373);
#6228=COLOUR_RGB('Dark Blue',0.08,0.2,0.34);
#6229=FILL_AREA_STYLE_COLOUR('',#6228);
#6230=FILL_AREA_STYLE('',(#6229));
#6231=SURFACE_STYLE_FILL_AREA(#6230);
#6232=SURFACE_SIDE_STYLE('',(#6231));
#6233=SURFACE_STYLE_USAGE(.BOTH.,#6232);
#6234=PRESENTATION_STYLE_ASSIGNMENT((#6233));
#6235=COLOUR_RGB('Light Blue',0.38,0.62,0.78);
#6236=FILL_AREA_STYLE_COLOUR('',#6235);
#6237=FILL_AREA_STYLE('',(#6236));
#6238=SURFACE_STYLE_FILL_AREA(#6237);
#6239=SURFACE_SIDE_STYLE('',(#6238));
#6240=SURFACE_STYLE_USAGE(.BOTH.,#6239);
#6241=PRESENTATION_STYLE_ASSIGNMENT((#6240));
#6242=COLOUR_RGB('Sky Blue',0.24,0.69,0.87);
#6243=FILL_AREA_STYLE_COLOUR('',#6242);
#6244=FILL_AREA_STYLE('',(#6243));
#6245=SURFACE_STYLE_FILL_AREA(#6244);
#6246=SURFACE_SIDE_STYLE('',(#6245));
#6247=SURFACE_STYLE_USAGE(.BOTH.,#6246);
#6248=PRESENTATION_STYLE_ASSIGNMENT((#6247));
#6249=COLOUR_RGB('Grey',0.48,0.52,0.57);
#6250=FILL_AREA_STYLE_COLOUR('',#6249);
#6251=FILL_AREA_STYLE('',(#6250));
#6252=SURFACE_STYLE_FILL_AREA(#6251);
#6253=SURFACE_SIDE_STYLE('',(#6252));
#6254=SURFACE_STYLE_USAGE(.BOTH.,#6253);
#6255=PRESENTATION_STYLE_ASSIGNMENT((#6254));
#6256=COLOUR_RGB('Black',0.12,0.14,0.17);
#6257=FILL_AREA_STYLE_COLOUR('',#6256);
#6258=FILL_AREA_STYLE('',(#6257));
#6259=SURFACE_STYLE_FILL_AREA(#6258);
#6260=SURFACE_SIDE_STYLE('',(#6259));
#6261=SURFACE_STYLE_USAGE(.BOTH.,#6260);
#6262=PRESENTATION_STYLE_ASSIGNMENT((#6261));
#6263=COLOUR_RGB('Off White',0.89,0.88,0.83);
#6264=FILL_AREA_STYLE_COLOUR('',#6263);
#6265=FILL_AREA_STYLE('',(#6264));
#6266=SURFACE_STYLE_FILL_AREA(#6265);
#6267=SURFACE_SIDE_STYLE('',(#6266));
#6268=SURFACE_STYLE_USAGE(.BOTH.,#6267);
#6269=PRESENTATION_STYLE_ASSIGNMENT((#6268));
ENDSEC;
END-ISO-10303-21;
